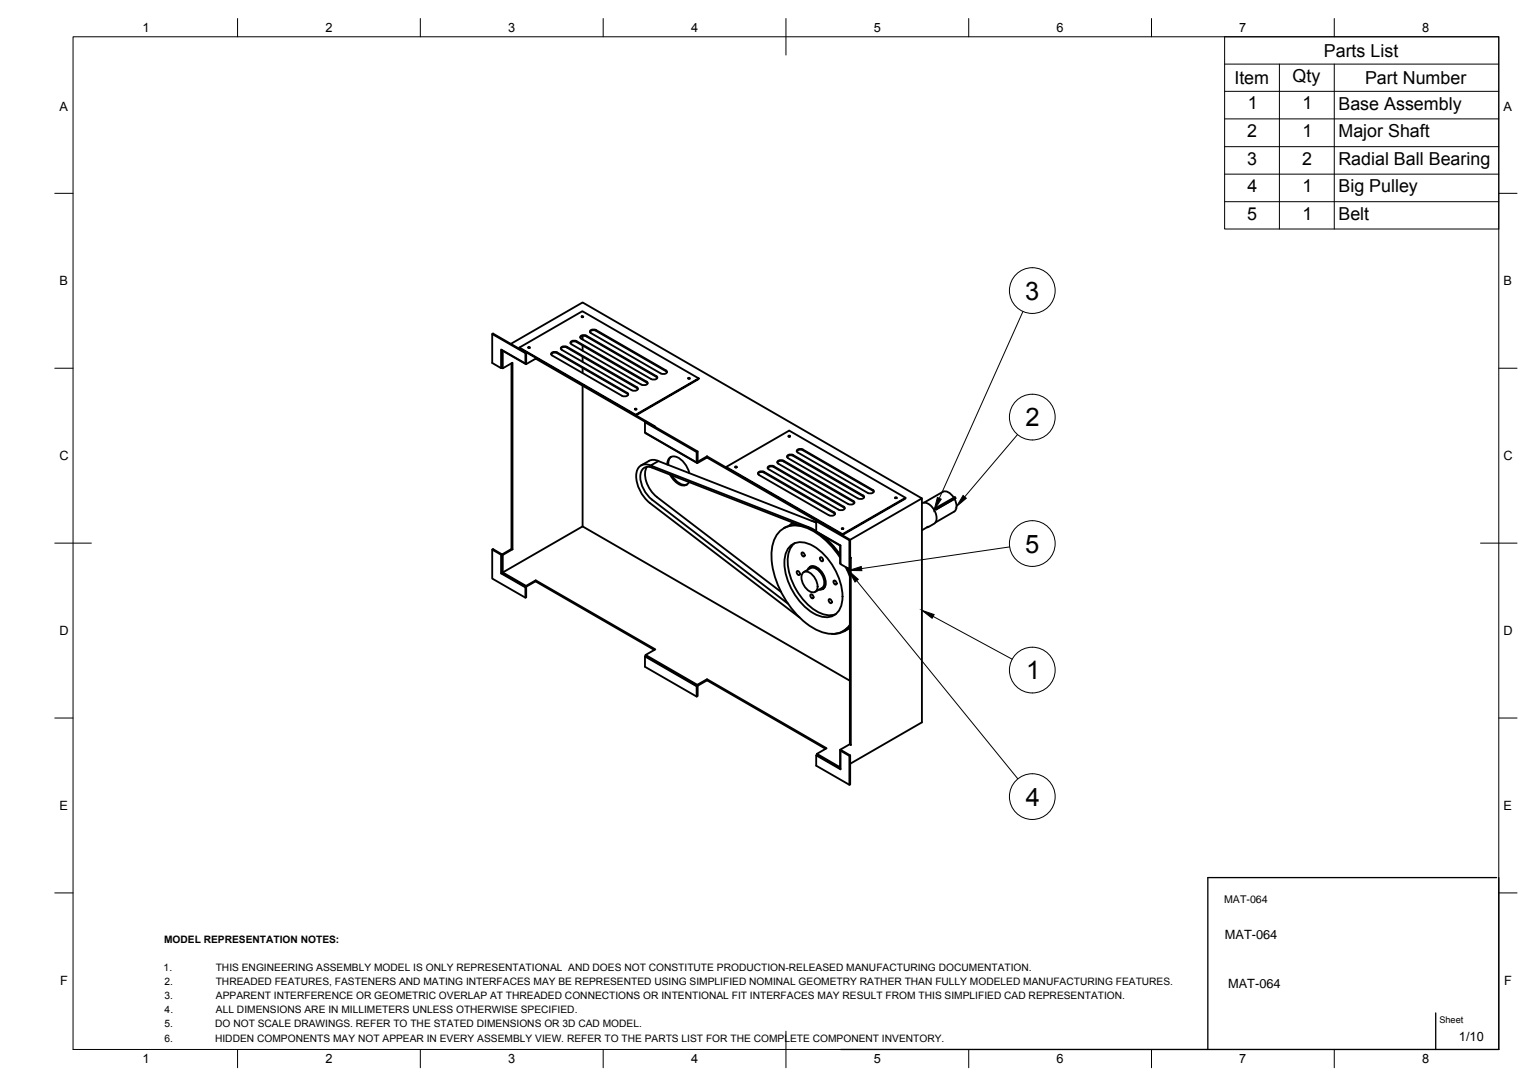
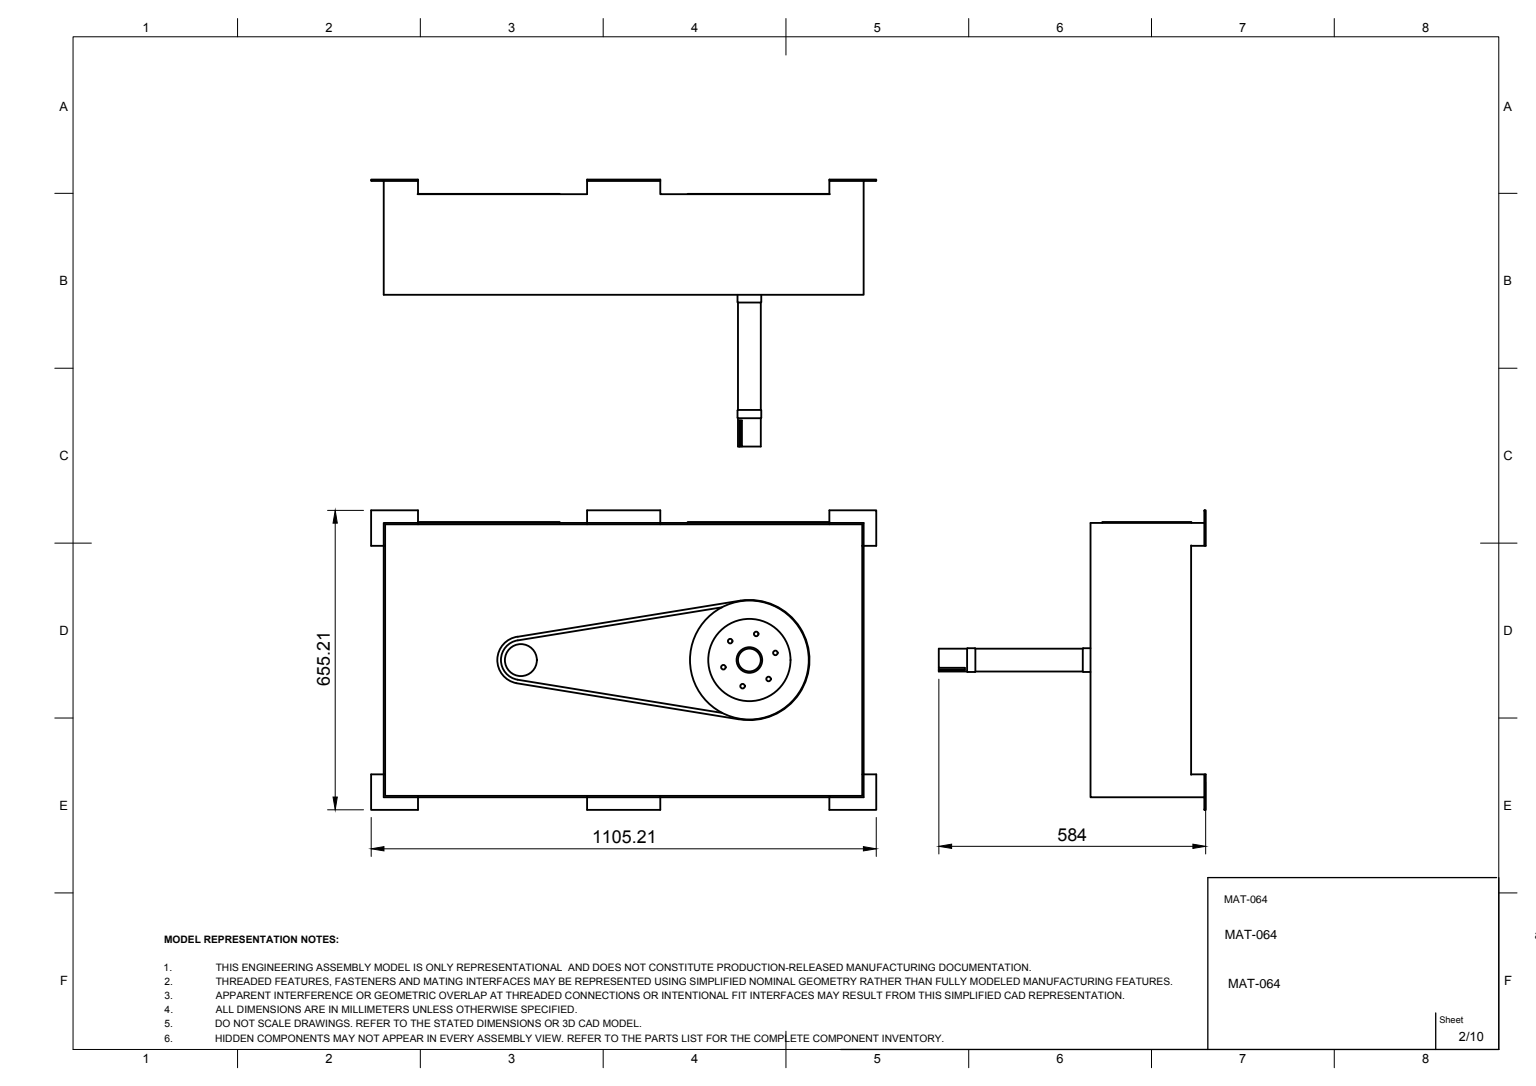
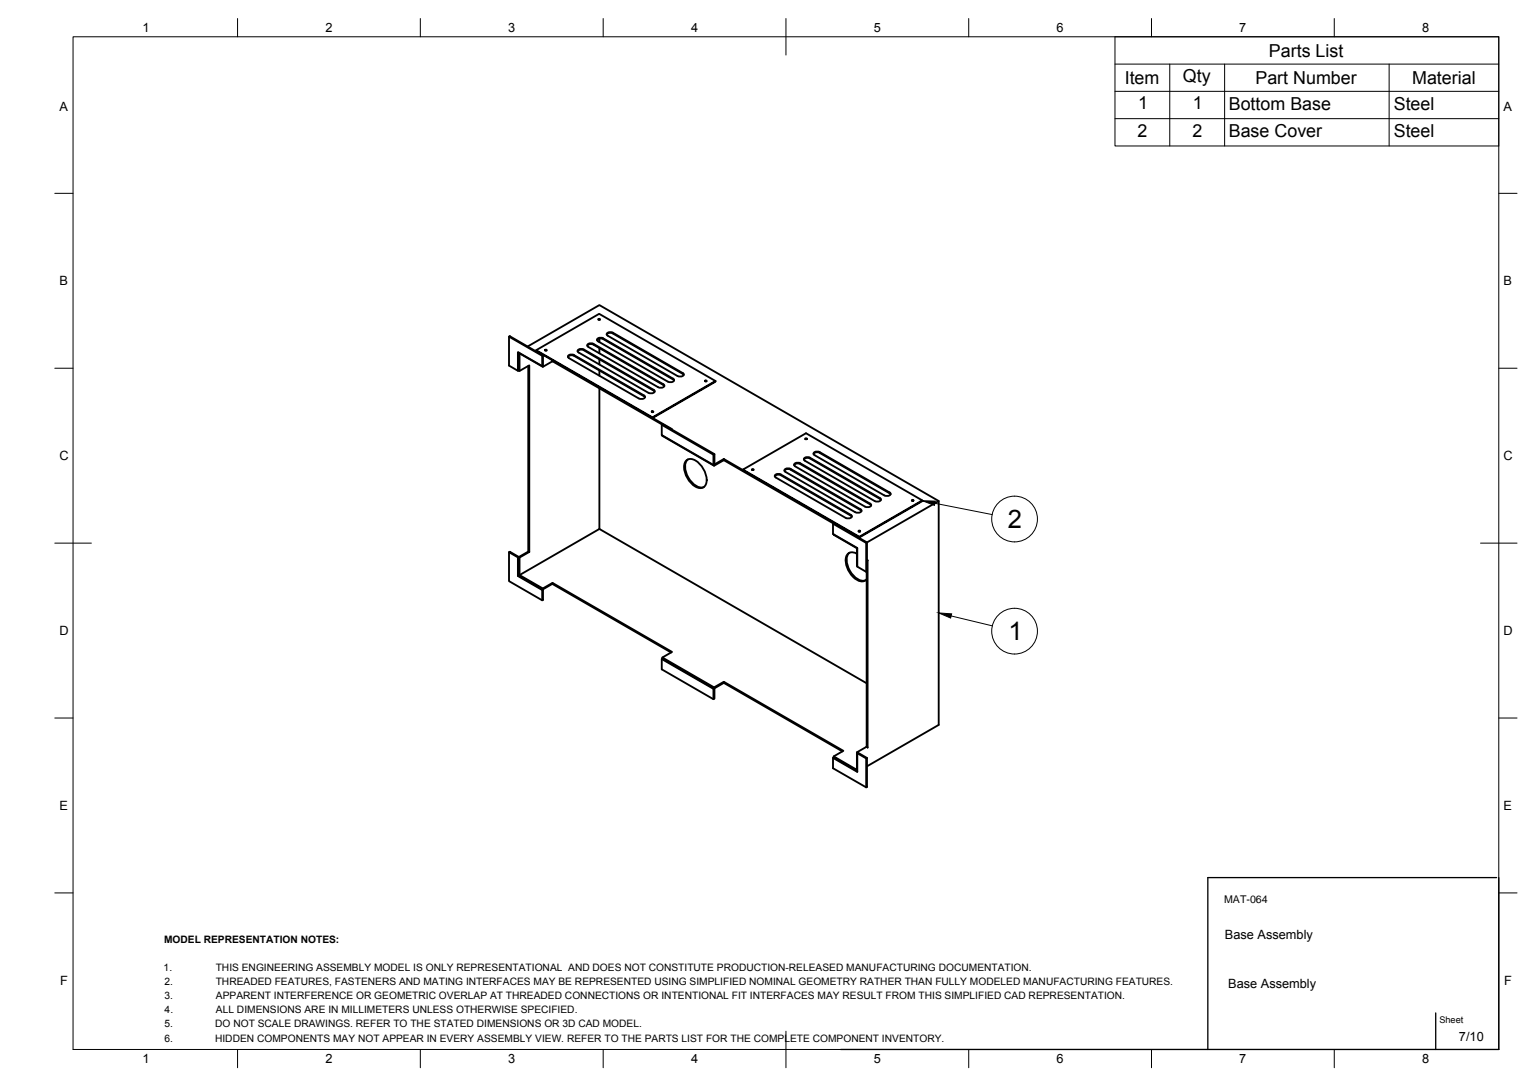
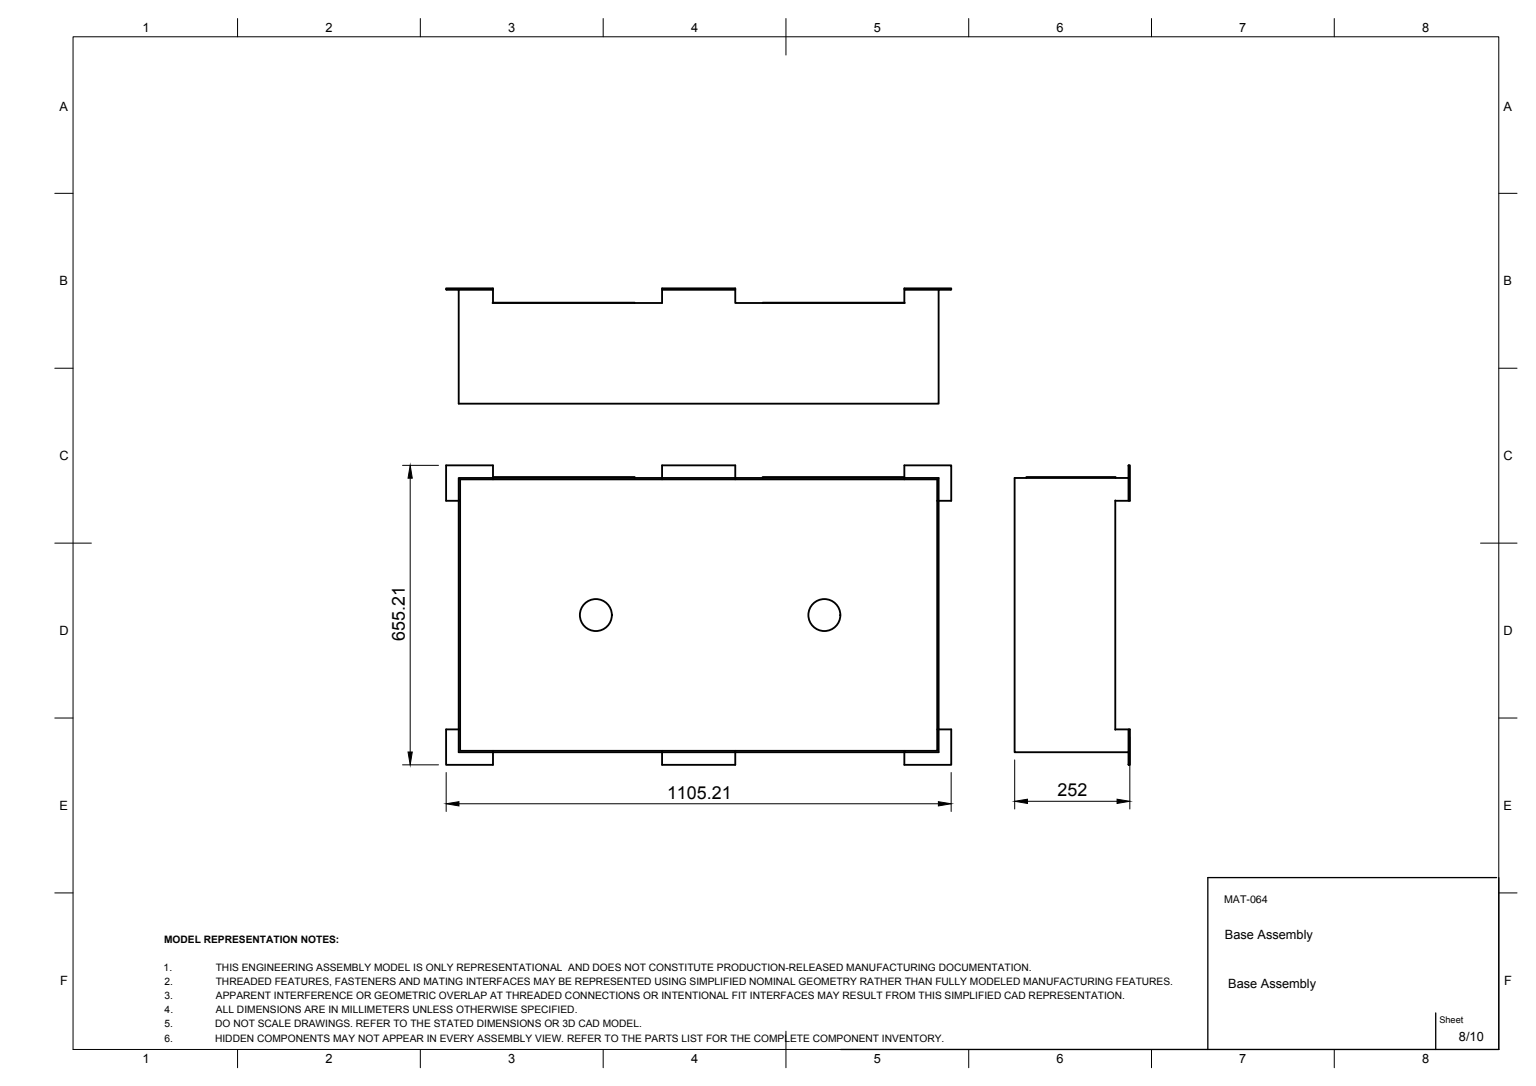
ISO-10303-21;
HEADER;
/* Generated by software containing ST-Developer
 * from STEP Tools, Inc. (www.steptools.com) 
 */

FILE_DESCRIPTION(
/* description */ (''),
/* implementation_level */ '2;1');

FILE_NAME(
/* name */ 
'MAT-064',
/* time_stamp */ '2026-10-24T12:42:14-07:00',
/* author */ (''),
/* organization */ (''),
/* preprocessor_version */ 'ST-DEVELOPER v20.2',
/* originating_system */ 'Autodesk Translation Framework v15.15.0.0',
/* authorisation */ '');

FILE_SCHEMA (('AUTOMOTIVE_DESIGN { 1 0 10303 214 3 1 1 }'));
ENDSEC;

DATA;
#10=MECHANICAL_DESIGN_GEOMETRIC_PRESENTATION_REPRESENTATION('',(#66,#67,
#68,#69,#70,#71),#6789);
#11=(
BOUNDED_SURFACE()
B_SPLINE_SURFACE(1,3,((#6689,#6690,#6691,#6692),(#6693,#6694,#6695,#6696)),
 .UNSPECIFIED.,.F.,.F.,.F.)
B_SPLINE_SURFACE_WITH_KNOTS((2,2),(4,4),(0.,1.),(0.,1.),.UNSPECIFIED.)
GEOMETRIC_REPRESENTATION_ITEM()
RATIONAL_B_SPLINE_SURFACE(((1.,0.44,0.44,1.),(1.,0.44,0.44,1.)))
REPRESENTATION_ITEM('')
SURFACE()
);
#12=(
BOUNDED_SURFACE()
B_SPLINE_SURFACE(1,3,((#6704,#6705,#6706,#6707),(#6708,#6709,#6710,#6711)),
 .UNSPECIFIED.,.F.,.F.,.F.)
B_SPLINE_SURFACE_WITH_KNOTS((2,2),(4,4),(0.,1.),(0.,1.),.UNSPECIFIED.)
GEOMETRIC_REPRESENTATION_ITEM()
RATIONAL_B_SPLINE_SURFACE(((1.,0.44,0.44,1.),(1.,0.44,0.44,1.)))
REPRESENTATION_ITEM('')
SURFACE()
);
#13=(
BOUNDED_SURFACE()
B_SPLINE_SURFACE(1,3,((#6733,#6734,#6735,#6736,#6737,#6738,#6739),(#6740,
#6741,#6742,#6743,#6744,#6745,#6746)),.UNSPECIFIED.,.F.,.F.,.F.)
B_SPLINE_SURFACE_WITH_KNOTS((2,2),(4,3,4),(0.,1.),(0.,0.5,1.),
 .UNSPECIFIED.)
GEOMETRIC_REPRESENTATION_ITEM()
RATIONAL_B_SPLINE_SURFACE(((1.,0.765382713227191,0.765382713227191,1.,0.765382713227191,
0.765382713227191,1.),(1.,0.765382713227191,0.765382713227191,1.,0.765382713227191,
0.765382713227191,1.)))
REPRESENTATION_ITEM('')
SURFACE()
);
#14=(
BOUNDED_SURFACE()
B_SPLINE_SURFACE(1,3,((#6750,#6751,#6752,#6753,#6754,#6755,#6756),(#6757,
#6758,#6759,#6760,#6761,#6762,#6763)),.UNSPECIFIED.,.F.,.F.,.F.)
B_SPLINE_SURFACE_WITH_KNOTS((2,2),(4,3,4),(0.,1.),(0.,0.5,1.),
 .UNSPECIFIED.)
GEOMETRIC_REPRESENTATION_ITEM()
RATIONAL_B_SPLINE_SURFACE(((1.,0.765382713227191,0.765382713227191,1.,0.765382713227191,
0.765382713227191,1.),(1.,0.765382713227191,0.765382713227191,1.,0.765382713227191,
0.765382713227191,1.)))
REPRESENTATION_ITEM('')
SURFACE()
);
#15=CONICAL_SURFACE('',#4306,7.5,0.0872664625997165);
#16=CONICAL_SURFACE('',#4399,122.,1.04719755119659);
#17=CONICAL_SURFACE('',#4402,130.,1.04719755119659);
#18=ITEM_DEFINED_TRANSFORMATION($,$,#4036,#4284);
#19=ITEM_DEFINED_TRANSFORMATION($,$,#4225,#4285);
#20=ITEM_DEFINED_TRANSFORMATION($,$,#4225,#4286);
#21=ITEM_DEFINED_TRANSFORMATION($,$,#4035,#4426);
#22=ITEM_DEFINED_TRANSFORMATION($,$,#4287,#4427);
#23=ITEM_DEFINED_TRANSFORMATION($,$,#4309,#4428);
#24=ITEM_DEFINED_TRANSFORMATION($,$,#4309,#4429);
#25=ITEM_DEFINED_TRANSFORMATION($,$,#4352,#4430);
#26=ITEM_DEFINED_TRANSFORMATION($,$,#4405,#4431);
#27=(
REPRESENTATION_RELATIONSHIP($,$,#6821,#6820)
REPRESENTATION_RELATIONSHIP_WITH_TRANSFORMATION(#18)
SHAPE_REPRESENTATION_RELATIONSHIP()
);
#28=(
REPRESENTATION_RELATIONSHIP($,$,#6822,#6820)
REPRESENTATION_RELATIONSHIP_WITH_TRANSFORMATION(#19)
SHAPE_REPRESENTATION_RELATIONSHIP()
);
#29=(
REPRESENTATION_RELATIONSHIP($,$,#6822,#6820)
REPRESENTATION_RELATIONSHIP_WITH_TRANSFORMATION(#20)
SHAPE_REPRESENTATION_RELATIONSHIP()
);
#30=(
REPRESENTATION_RELATIONSHIP($,$,#6820,#6819)
REPRESENTATION_RELATIONSHIP_WITH_TRANSFORMATION(#21)
SHAPE_REPRESENTATION_RELATIONSHIP()
);
#31=(
REPRESENTATION_RELATIONSHIP($,$,#6823,#6819)
REPRESENTATION_RELATIONSHIP_WITH_TRANSFORMATION(#22)
SHAPE_REPRESENTATION_RELATIONSHIP()
);
#32=(
REPRESENTATION_RELATIONSHIP($,$,#6824,#6819)
REPRESENTATION_RELATIONSHIP_WITH_TRANSFORMATION(#23)
SHAPE_REPRESENTATION_RELATIONSHIP()
);
#33=(
REPRESENTATION_RELATIONSHIP($,$,#6824,#6819)
REPRESENTATION_RELATIONSHIP_WITH_TRANSFORMATION(#24)
SHAPE_REPRESENTATION_RELATIONSHIP()
);
#34=(
REPRESENTATION_RELATIONSHIP($,$,#6825,#6819)
REPRESENTATION_RELATIONSHIP_WITH_TRANSFORMATION(#25)
SHAPE_REPRESENTATION_RELATIONSHIP()
);
#35=(
REPRESENTATION_RELATIONSHIP($,$,#6826,#6819)
REPRESENTATION_RELATIONSHIP_WITH_TRANSFORMATION(#26)
SHAPE_REPRESENTATION_RELATIONSHIP()
);
#36=CONTEXT_DEPENDENT_SHAPE_REPRESENTATION(#27,#6806);
#37=CONTEXT_DEPENDENT_SHAPE_REPRESENTATION(#28,#6807);
#38=CONTEXT_DEPENDENT_SHAPE_REPRESENTATION(#29,#6808);
#39=CONTEXT_DEPENDENT_SHAPE_REPRESENTATION(#30,#6813);
#40=CONTEXT_DEPENDENT_SHAPE_REPRESENTATION(#31,#6814);
#41=CONTEXT_DEPENDENT_SHAPE_REPRESENTATION(#32,#6815);
#42=CONTEXT_DEPENDENT_SHAPE_REPRESENTATION(#33,#6816);
#43=CONTEXT_DEPENDENT_SHAPE_REPRESENTATION(#34,#6817);
#44=CONTEXT_DEPENDENT_SHAPE_REPRESENTATION(#35,#6818);
#45=NEXT_ASSEMBLY_USAGE_OCCURRENCE('Bottom Base:1','Bottom Base:1',
'Bottom Base:1',#6829,#6830,'Bottom Base:1');
#46=NEXT_ASSEMBLY_USAGE_OCCURRENCE('Base Cover:1','Base Cover:1',
'Base Cover:1',#6829,#6831,'Base Cover:1');
#47=NEXT_ASSEMBLY_USAGE_OCCURRENCE('Base Cover:2','Base Cover:2',
'Base Cover:2',#6829,#6831,'Base Cover:2');
#48=NEXT_ASSEMBLY_USAGE_OCCURRENCE('Base Assembly:1','Base Assembly:1',
'Base Assembly:1',#6828,#6829,'Base Assembly:1');
#49=NEXT_ASSEMBLY_USAGE_OCCURRENCE('Major Shaft:1','Major Shaft:1',
'Major Shaft:1',#6828,#6832,'Major Shaft:1');
#50=NEXT_ASSEMBLY_USAGE_OCCURRENCE('Radial Ball Bearing:1',
'Radial Ball Bearing:1','Radial Ball Bearing:1',#6828,#6833,
'Radial Ball Bearing:1');
#51=NEXT_ASSEMBLY_USAGE_OCCURRENCE('Radial Ball Bearing:2',
'Radial Ball Bearing:2','Radial Ball Bearing:2',#6828,#6833,
'Radial Ball Bearing:2');
#52=NEXT_ASSEMBLY_USAGE_OCCURRENCE('Big Pulley:1','Big Pulley:1',
'Big Pulley:1',#6828,#6834,'Big Pulley:1');
#53=NEXT_ASSEMBLY_USAGE_OCCURRENCE('Belt:1','Belt:1','Belt:1',#6828,#6835,
'Belt:1');
#54=SHAPE_REPRESENTATION_RELATIONSHIP('SRR','None',#6821,#60);
#55=SHAPE_REPRESENTATION_RELATIONSHIP('SRR','None',#6822,#61);
#56=SHAPE_REPRESENTATION_RELATIONSHIP('SRR','None',#6823,#62);
#57=SHAPE_REPRESENTATION_RELATIONSHIP('SRR','None',#6824,#63);
#58=SHAPE_REPRESENTATION_RELATIONSHIP('SRR','None',#6825,#64);
#59=SHAPE_REPRESENTATION_RELATIONSHIP('SRR','None',#6826,#65);
#60=ADVANCED_BREP_SHAPE_REPRESENTATION('',(#72),#6783);
#61=ADVANCED_BREP_SHAPE_REPRESENTATION('',(#73),#6784);
#62=ADVANCED_BREP_SHAPE_REPRESENTATION('',(#74),#6785);
#63=ADVANCED_BREP_SHAPE_REPRESENTATION('',(#75),#6786);
#64=ADVANCED_BREP_SHAPE_REPRESENTATION('',(#76),#6787);
#65=ADVANCED_BREP_SHAPE_REPRESENTATION('',(#77),#6788);
#66=STYLED_ITEM('',(#6863),#72);
#67=STYLED_ITEM('',(#6863),#73);
#68=STYLED_ITEM('',(#6863),#74);
#69=STYLED_ITEM('',(#6863),#75);
#70=STYLED_ITEM('',(#6864),#76);
#71=STYLED_ITEM('',(#6863),#77);
#72=MANIFOLD_SOLID_BREP('Bottom Base',#3961);
#73=MANIFOLD_SOLID_BREP('Base Cover',#3962);
#74=MANIFOLD_SOLID_BREP('Major Shaft',#3963);
#75=MANIFOLD_SOLID_BREP('Radial Ball Bearing',#3964);
#76=MANIFOLD_SOLID_BREP('Big Pulley',#3965);
#77=MANIFOLD_SOLID_BREP('Belt',#3966);
#78=TOROIDAL_SURFACE('',#4150,2.,1.);
#79=TOROIDAL_SURFACE('',#4160,2.,1.);
#80=TOROIDAL_SURFACE('',#4170,2.,1.);
#81=TOROIDAL_SURFACE('',#4180,2.,1.);
#82=TOROIDAL_SURFACE('',#4190,2.,1.);
#83=TOROIDAL_SURFACE('',#4200,2.,1.);
#84=TOROIDAL_SURFACE('',#4208,2.,1.);
#85=TOROIDAL_SURFACE('',#4220,2.,1.);
#86=TOROIDAL_SURFACE('',#4310,19.25,4.05);
#87=TOROIDAL_SURFACE('',#4324,13.5,1.);
#88=TOROIDAL_SURFACE('',#4329,13.5,1.);
#89=TOROIDAL_SURFACE('',#4333,19.25,4.05);
#90=TOROIDAL_SURFACE('',#4343,25.,0.999999999999999);
#91=TOROIDAL_SURFACE('',#4348,25.,0.999999999999999);
#92=ELLIPSE('',#4145,1.41421356237309,1.);
#93=ELLIPSE('',#4149,1.41421356237309,1.);
#94=ELLIPSE('',#4153,1.41421356237309,1.);
#95=ELLIPSE('',#4155,1.41421356237309,1.);
#96=ELLIPSE('',#4165,1.4142135623731,1.);
#97=ELLIPSE('',#4169,1.41421356237309,1.);
#98=ELLIPSE('',#4173,1.41421356237309,1.);
#99=ELLIPSE('',#4175,1.41421356237309,1.);
#100=ELLIPSE('',#4185,1.41421356237309,1.);
#101=ELLIPSE('',#4189,1.41421356237309,1.);
#102=ELLIPSE('',#4193,1.41421356237309,1.);
#103=ELLIPSE('',#4195,1.41421356237309,1.);
#104=ELLIPSE('',#4206,1.41421356237309,1.);
#105=ELLIPSE('',#4211,1.41421356237309,1.);
#106=ELLIPSE('',#4213,1.4142135623731,1.);
#107=ELLIPSE('',#4215,1.4142135623731,1.);
#108=CYLINDRICAL_SURFACE('',#4093,2.);
#109=CYLINDRICAL_SURFACE('',#4094,2.);
#110=CYLINDRICAL_SURFACE('',#4095,2.);
#111=CYLINDRICAL_SURFACE('',#4096,2.);
#112=CYLINDRICAL_SURFACE('',#4143,1.);
#113=CYLINDRICAL_SURFACE('',#4146,1.);
#114=CYLINDRICAL_SURFACE('',#4148,1.);
#115=CYLINDRICAL_SURFACE('',#4152,1.);
#116=CYLINDRICAL_SURFACE('',#4154,1.);
#117=CYLINDRICAL_SURFACE('',#4156,1.);
#118=CYLINDRICAL_SURFACE('',#4158,1.);
#119=CYLINDRICAL_SURFACE('',#4162,1.);
#120=CYLINDRICAL_SURFACE('',#4163,1.);
#121=CYLINDRICAL_SURFACE('',#4166,1.);
#122=CYLINDRICAL_SURFACE('',#4168,1.);
#123=CYLINDRICAL_SURFACE('',#4172,1.);
#124=CYLINDRICAL_SURFACE('',#4174,1.);
#125=CYLINDRICAL_SURFACE('',#4176,1.);
#126=CYLINDRICAL_SURFACE('',#4178,1.);
#127=CYLINDRICAL_SURFACE('',#4182,1.);
#128=CYLINDRICAL_SURFACE('',#4183,1.);
#129=CYLINDRICAL_SURFACE('',#4186,1.);
#130=CYLINDRICAL_SURFACE('',#4188,1.);
#131=CYLINDRICAL_SURFACE('',#4192,1.);
#132=CYLINDRICAL_SURFACE('',#4194,1.);
#133=CYLINDRICAL_SURFACE('',#4196,1.);
#134=CYLINDRICAL_SURFACE('',#4198,1.);
#135=CYLINDRICAL_SURFACE('',#4202,1.);
#136=CYLINDRICAL_SURFACE('',#4203,1.);
#137=CYLINDRICAL_SURFACE('',#4205,1.);
#138=CYLINDRICAL_SURFACE('',#4210,1.);
#139=CYLINDRICAL_SURFACE('',#4212,1.);
#140=CYLINDRICAL_SURFACE('',#4214,1.);
#141=CYLINDRICAL_SURFACE('',#4216,1.);
#142=CYLINDRICAL_SURFACE('',#4218,1.);
#143=CYLINDRICAL_SURFACE('',#4222,1.);
#144=CYLINDRICAL_SURFACE('',#4223,35.);
#145=CYLINDRICAL_SURFACE('',#4224,35.);
#146=CYLINDRICAL_SURFACE('',#4260,2.);
#147=CYLINDRICAL_SURFACE('',#4261,2.);
#148=CYLINDRICAL_SURFACE('',#4262,2.);
#149=CYLINDRICAL_SURFACE('',#4263,2.);
#150=CYLINDRICAL_SURFACE('',#4264,7.99999999999998);
#151=CYLINDRICAL_SURFACE('',#4266,8.00000000000009);
#152=CYLINDRICAL_SURFACE('',#4268,8.00000000000009);
#153=CYLINDRICAL_SURFACE('',#4270,8.00000000000004);
#154=CYLINDRICAL_SURFACE('',#4272,7.99999999999998);
#155=CYLINDRICAL_SURFACE('',#4274,8.00000000000009);
#156=CYLINDRICAL_SURFACE('',#4276,8.00000000000009);
#157=CYLINDRICAL_SURFACE('',#4278,8.00000000000004);
#158=CYLINDRICAL_SURFACE('',#4280,8.00000000000004);
#159=CYLINDRICAL_SURFACE('',#4282,8.00000000000004);
#160=CYLINDRICAL_SURFACE('',#4288,25.);
#161=CYLINDRICAL_SURFACE('',#4316,16.55);
#162=CYLINDRICAL_SURFACE('',#4318,16.55);
#163=CYLINDRICAL_SURFACE('',#4327,12.5);
#164=CYLINDRICAL_SURFACE('',#4337,21.95);
#165=CYLINDRICAL_SURFACE('',#4339,21.95);
#166=CYLINDRICAL_SURFACE('',#4346,26.);
#167=CYLINDRICAL_SURFACE('',#4353,130.);
#168=CYLINDRICAL_SURFACE('',#4356,130.);
#169=CYLINDRICAL_SURFACE('',#4360,5.);
#170=CYLINDRICAL_SURFACE('',#4363,5.);
#171=CYLINDRICAL_SURFACE('',#4366,5.);
#172=CYLINDRICAL_SURFACE('',#4369,5.);
#173=CYLINDRICAL_SURFACE('',#4372,5.);
#174=CYLINDRICAL_SURFACE('',#4375,90.);
#175=CYLINDRICAL_SURFACE('',#4378,90.);
#176=CYLINDRICAL_SURFACE('',#4389,28.);
#177=CYLINDRICAL_SURFACE('',#4391,25.);
#178=CYLINDRICAL_SURFACE('',#4394,28.);
#179=CYLINDRICAL_SURFACE('',#4398,5.);
#180=CYLINDRICAL_SURFACE('',#4404,122.);
#181=CYLINDRICAL_SURFACE('',#4409,51.471200702168);
#182=CYLINDRICAL_SURFACE('',#4413,43.5522017822105);
#183=CYLINDRICAL_SURFACE('',#4419,131.457333002004);
#184=CYLINDRICAL_SURFACE('',#4423,123.55173167544);
#185=FACE_BOUND('',#612,.T.);
#186=FACE_BOUND('',#613,.T.);
#187=FACE_BOUND('',#614,.T.);
#188=FACE_BOUND('',#615,.T.);
#189=FACE_BOUND('',#616,.T.);
#190=FACE_BOUND('',#617,.T.);
#191=FACE_BOUND('',#624,.T.);
#192=FACE_BOUND('',#625,.T.);
#193=FACE_BOUND('',#626,.T.);
#194=FACE_BOUND('',#627,.T.);
#195=FACE_BOUND('',#628,.T.);
#196=FACE_BOUND('',#629,.T.);
#197=FACE_BOUND('',#635,.T.);
#198=FACE_BOUND('',#636,.T.);
#199=FACE_BOUND('',#641,.T.);
#200=FACE_BOUND('',#642,.T.);
#201=FACE_BOUND('',#752,.T.);
#202=FACE_BOUND('',#753,.T.);
#203=FACE_BOUND('',#754,.T.);
#204=FACE_BOUND('',#755,.T.);
#205=FACE_BOUND('',#756,.T.);
#206=FACE_BOUND('',#757,.T.);
#207=FACE_BOUND('',#758,.T.);
#208=FACE_BOUND('',#759,.T.);
#209=FACE_BOUND('',#760,.T.);
#210=FACE_BOUND('',#762,.T.);
#211=FACE_BOUND('',#763,.T.);
#212=FACE_BOUND('',#764,.T.);
#213=FACE_BOUND('',#765,.T.);
#214=FACE_BOUND('',#766,.T.);
#215=FACE_BOUND('',#767,.T.);
#216=FACE_BOUND('',#768,.T.);
#217=FACE_BOUND('',#769,.T.);
#218=FACE_BOUND('',#770,.T.);
#219=FACE_BOUND('',#797,.T.);
#220=FACE_BOUND('',#813,.T.);
#221=FACE_BOUND('',#818,.T.);
#222=FACE_BOUND('',#823,.T.);
#223=FACE_BOUND('',#828,.T.);
#224=FACE_BOUND('',#839,.T.);
#225=FACE_BOUND('',#841,.T.);
#226=FACE_BOUND('',#843,.T.);
#227=FACE_BOUND('',#844,.T.);
#228=FACE_BOUND('',#845,.T.);
#229=FACE_BOUND('',#846,.T.);
#230=FACE_BOUND('',#847,.T.);
#231=FACE_BOUND('',#848,.T.);
#232=FACE_BOUND('',#849,.T.);
#233=FACE_BOUND('',#851,.T.);
#234=FACE_BOUND('',#852,.T.);
#235=FACE_BOUND('',#853,.T.);
#236=FACE_BOUND('',#854,.T.);
#237=FACE_BOUND('',#855,.T.);
#238=FACE_BOUND('',#856,.T.);
#239=FACE_BOUND('',#857,.T.);
#240=FACE_BOUND('',#862,.T.);
#241=FACE_BOUND('',#864,.T.);
#242=CIRCLE('',#4038,2.);
#243=CIRCLE('',#4039,2.);
#244=CIRCLE('',#4040,2.);
#245=CIRCLE('',#4041,2.);
#246=CIRCLE('',#4048,2.);
#247=CIRCLE('',#4049,2.);
#248=CIRCLE('',#4050,2.);
#249=CIRCLE('',#4051,2.);
#250=CIRCLE('',#4057,35.);
#251=CIRCLE('',#4058,35.);
#252=CIRCLE('',#4063,35.);
#253=CIRCLE('',#4064,35.);
#254=CIRCLE('',#4067,1.);
#255=CIRCLE('',#4069,2.);
#256=CIRCLE('',#4071,2.);
#257=CIRCLE('',#4073,1.);
#258=CIRCLE('',#4077,1.);
#259=CIRCLE('',#4079,2.);
#260=CIRCLE('',#4082,2.);
#261=CIRCLE('',#4084,1.);
#262=CIRCLE('',#4098,2.);
#263=CIRCLE('',#4100,1.);
#264=CIRCLE('',#4101,1.);
#265=CIRCLE('',#4103,2.);
#266=CIRCLE('',#4105,2.);
#267=CIRCLE('',#4107,1.);
#268=CIRCLE('',#4108,1.);
#269=CIRCLE('',#4110,2.);
#270=CIRCLE('',#4144,1.);
#271=CIRCLE('',#4147,1.);
#272=CIRCLE('',#4151,1.);
#273=CIRCLE('',#4157,1.);
#274=CIRCLE('',#4159,1.);
#275=CIRCLE('',#4161,1.);
#276=CIRCLE('',#4164,1.);
#277=CIRCLE('',#4167,1.);
#278=CIRCLE('',#4171,1.);
#279=CIRCLE('',#4177,1.);
#280=CIRCLE('',#4179,1.);
#281=CIRCLE('',#4181,1.);
#282=CIRCLE('',#4184,1.);
#283=CIRCLE('',#4187,1.);
#284=CIRCLE('',#4191,1.);
#285=CIRCLE('',#4197,1.);
#286=CIRCLE('',#4199,1.);
#287=CIRCLE('',#4201,1.);
#288=CIRCLE('',#4204,1.);
#289=CIRCLE('',#4207,1.);
#290=CIRCLE('',#4209,1.);
#291=CIRCLE('',#4217,1.);
#292=CIRCLE('',#4219,1.);
#293=CIRCLE('',#4221,1.);
#294=CIRCLE('',#4231,8.00000000000004);
#295=CIRCLE('',#4232,8.00000000000004);
#296=CIRCLE('',#4233,8.00000000000009);
#297=CIRCLE('',#4234,8.00000000000004);
#298=CIRCLE('',#4235,7.99999999999998);
#299=CIRCLE('',#4236,8.00000000000009);
#300=CIRCLE('',#4237,8.00000000000009);
#301=CIRCLE('',#4238,8.00000000000004);
#302=CIRCLE('',#4239,7.99999999999998);
#303=CIRCLE('',#4240,8.00000000000009);
#304=CIRCLE('',#4241,2.);
#305=CIRCLE('',#4242,2.);
#306=CIRCLE('',#4243,2.);
#307=CIRCLE('',#4244,2.);
#308=CIRCLE('',#4246,8.00000000000004);
#309=CIRCLE('',#4247,8.00000000000004);
#310=CIRCLE('',#4248,8.00000000000009);
#311=CIRCLE('',#4249,8.00000000000004);
#312=CIRCLE('',#4250,7.99999999999998);
#313=CIRCLE('',#4251,8.00000000000009);
#314=CIRCLE('',#4252,8.00000000000009);
#315=CIRCLE('',#4253,8.00000000000004);
#316=CIRCLE('',#4254,7.99999999999998);
#317=CIRCLE('',#4255,8.00000000000009);
#318=CIRCLE('',#4256,2.);
#319=CIRCLE('',#4257,2.);
#320=CIRCLE('',#4258,2.);
#321=CIRCLE('',#4259,2.);
#322=CIRCLE('',#4289,25.);
#323=CIRCLE('',#4290,25.);
#324=CIRCLE('',#4291,25.);
#325=CIRCLE('',#4292,25.);
#326=CIRCLE('',#4293,25.);
#327=CIRCLE('',#4294,25.);
#328=CIRCLE('',#4296,7.5);
#329=CIRCLE('',#4307,4.87534009422228);
#330=CIRCLE('',#4311,21.95);
#331=CIRCLE('',#4312,4.05);
#332=CIRCLE('',#4313,16.55);
#333=CIRCLE('',#4314,16.55);
#334=CIRCLE('',#4315,21.95);
#335=CIRCLE('',#4317,16.55);
#336=CIRCLE('',#4319,16.55);
#337=CIRCLE('',#4320,16.55);
#338=CIRCLE('',#4321,16.55);
#339=CIRCLE('',#4323,13.5);
#340=CIRCLE('',#4325,12.5);
#341=CIRCLE('',#4326,1.);
#342=CIRCLE('',#4328,12.5);
#343=CIRCLE('',#4330,13.5);
#344=CIRCLE('',#4331,1.);
#345=CIRCLE('',#4334,4.05);
#346=CIRCLE('',#4335,21.95);
#347=CIRCLE('',#4336,21.95);
#348=CIRCLE('',#4338,21.95);
#349=CIRCLE('',#4340,21.95);
#350=CIRCLE('',#4342,25.);
#351=CIRCLE('',#4344,0.999999999999999);
#352=CIRCLE('',#4345,26.);
#353=CIRCLE('',#4347,26.);
#354=CIRCLE('',#4349,0.999999999999999);
#355=CIRCLE('',#4350,25.);
#356=CIRCLE('',#4354,130.);
#357=CIRCLE('',#4355,130.);
#358=CIRCLE('',#4357,130.);
#359=CIRCLE('',#4358,130.);
#360=CIRCLE('',#4359,130.);
#361=CIRCLE('',#4361,5.);
#362=CIRCLE('',#4362,5.);
#363=CIRCLE('',#4364,5.);
#364=CIRCLE('',#4365,5.);
#365=CIRCLE('',#4367,5.);
#366=CIRCLE('',#4368,5.);
#367=CIRCLE('',#4370,5.);
#368=CIRCLE('',#4371,5.);
#369=CIRCLE('',#4373,5.);
#370=CIRCLE('',#4374,5.);
#371=CIRCLE('',#4376,90.);
#372=CIRCLE('',#4377,90.);
#373=CIRCLE('',#4379,90.);
#374=CIRCLE('',#4380,90.);
#375=CIRCLE('',#4384,5.);
#376=CIRCLE('',#4385,28.);
#377=CIRCLE('',#4387,5.);
#378=CIRCLE('',#4388,28.);
#379=CIRCLE('',#4390,28.);
#380=CIRCLE('',#4392,25.);
#381=CIRCLE('',#4393,25.);
#382=CIRCLE('',#4395,28.);
#383=CIRCLE('',#4400,122.);
#384=CIRCLE('',#4401,122.);
#385=CIRCLE('',#4403,122.);
#386=CIRCLE('',#4410,51.471200702168);
#387=CIRCLE('',#4411,51.471200702168);
#388=CIRCLE('',#4412,43.5522017822105);
#389=CIRCLE('',#4414,43.5522017822105);
#390=CIRCLE('',#4420,131.457333002004);
#391=CIRCLE('',#4421,131.457333002004);
#392=CIRCLE('',#4422,123.55173167544);
#393=CIRCLE('',#4424,123.55173167544);
#394=FACE_OUTER_BOUND('',#611,.T.);
#395=FACE_OUTER_BOUND('',#618,.T.);
#396=FACE_OUTER_BOUND('',#619,.T.);
#397=FACE_OUTER_BOUND('',#620,.T.);
#398=FACE_OUTER_BOUND('',#621,.T.);
#399=FACE_OUTER_BOUND('',#622,.T.);
#400=FACE_OUTER_BOUND('',#623,.T.);
#401=FACE_OUTER_BOUND('',#630,.T.);
#402=FACE_OUTER_BOUND('',#631,.T.);
#403=FACE_OUTER_BOUND('',#632,.T.);
#404=FACE_OUTER_BOUND('',#633,.T.);
#405=FACE_OUTER_BOUND('',#634,.T.);
#406=FACE_OUTER_BOUND('',#637,.T.);
#407=FACE_OUTER_BOUND('',#638,.T.);
#408=FACE_OUTER_BOUND('',#639,.T.);
#409=FACE_OUTER_BOUND('',#640,.T.);
#410=FACE_OUTER_BOUND('',#643,.T.);
#411=FACE_OUTER_BOUND('',#644,.T.);
#412=FACE_OUTER_BOUND('',#645,.T.);
#413=FACE_OUTER_BOUND('',#646,.T.);
#414=FACE_OUTER_BOUND('',#647,.T.);
#415=FACE_OUTER_BOUND('',#648,.T.);
#416=FACE_OUTER_BOUND('',#649,.T.);
#417=FACE_OUTER_BOUND('',#650,.T.);
#418=FACE_OUTER_BOUND('',#651,.T.);
#419=FACE_OUTER_BOUND('',#652,.T.);
#420=FACE_OUTER_BOUND('',#653,.T.);
#421=FACE_OUTER_BOUND('',#654,.T.);
#422=FACE_OUTER_BOUND('',#655,.T.);
#423=FACE_OUTER_BOUND('',#656,.T.);
#424=FACE_OUTER_BOUND('',#657,.T.);
#425=FACE_OUTER_BOUND('',#658,.T.);
#426=FACE_OUTER_BOUND('',#659,.T.);
#427=FACE_OUTER_BOUND('',#660,.T.);
#428=FACE_OUTER_BOUND('',#661,.T.);
#429=FACE_OUTER_BOUND('',#662,.T.);
#430=FACE_OUTER_BOUND('',#663,.T.);
#431=FACE_OUTER_BOUND('',#664,.T.);
#432=FACE_OUTER_BOUND('',#665,.T.);
#433=FACE_OUTER_BOUND('',#666,.T.);
#434=FACE_OUTER_BOUND('',#667,.T.);
#435=FACE_OUTER_BOUND('',#668,.T.);
#436=FACE_OUTER_BOUND('',#669,.T.);
#437=FACE_OUTER_BOUND('',#670,.T.);
#438=FACE_OUTER_BOUND('',#671,.T.);
#439=FACE_OUTER_BOUND('',#672,.T.);
#440=FACE_OUTER_BOUND('',#673,.T.);
#441=FACE_OUTER_BOUND('',#674,.T.);
#442=FACE_OUTER_BOUND('',#675,.T.);
#443=FACE_OUTER_BOUND('',#676,.T.);
#444=FACE_OUTER_BOUND('',#677,.T.);
#445=FACE_OUTER_BOUND('',#678,.T.);
#446=FACE_OUTER_BOUND('',#679,.T.);
#447=FACE_OUTER_BOUND('',#680,.T.);
#448=FACE_OUTER_BOUND('',#681,.T.);
#449=FACE_OUTER_BOUND('',#682,.T.);
#450=FACE_OUTER_BOUND('',#683,.T.);
#451=FACE_OUTER_BOUND('',#684,.T.);
#452=FACE_OUTER_BOUND('',#685,.T.);
#453=FACE_OUTER_BOUND('',#686,.T.);
#454=FACE_OUTER_BOUND('',#687,.T.);
#455=FACE_OUTER_BOUND('',#688,.T.);
#456=FACE_OUTER_BOUND('',#689,.T.);
#457=FACE_OUTER_BOUND('',#690,.T.);
#458=FACE_OUTER_BOUND('',#691,.T.);
#459=FACE_OUTER_BOUND('',#692,.T.);
#460=FACE_OUTER_BOUND('',#693,.T.);
#461=FACE_OUTER_BOUND('',#694,.T.);
#462=FACE_OUTER_BOUND('',#695,.T.);
#463=FACE_OUTER_BOUND('',#696,.T.);
#464=FACE_OUTER_BOUND('',#697,.T.);
#465=FACE_OUTER_BOUND('',#698,.T.);
#466=FACE_OUTER_BOUND('',#699,.T.);
#467=FACE_OUTER_BOUND('',#700,.T.);
#468=FACE_OUTER_BOUND('',#701,.T.);
#469=FACE_OUTER_BOUND('',#702,.T.);
#470=FACE_OUTER_BOUND('',#703,.T.);
#471=FACE_OUTER_BOUND('',#704,.T.);
#472=FACE_OUTER_BOUND('',#705,.T.);
#473=FACE_OUTER_BOUND('',#706,.T.);
#474=FACE_OUTER_BOUND('',#707,.T.);
#475=FACE_OUTER_BOUND('',#708,.T.);
#476=FACE_OUTER_BOUND('',#709,.T.);
#477=FACE_OUTER_BOUND('',#710,.T.);
#478=FACE_OUTER_BOUND('',#711,.T.);
#479=FACE_OUTER_BOUND('',#712,.T.);
#480=FACE_OUTER_BOUND('',#713,.T.);
#481=FACE_OUTER_BOUND('',#714,.T.);
#482=FACE_OUTER_BOUND('',#715,.T.);
#483=FACE_OUTER_BOUND('',#716,.T.);
#484=FACE_OUTER_BOUND('',#717,.T.);
#485=FACE_OUTER_BOUND('',#718,.T.);
#486=FACE_OUTER_BOUND('',#719,.T.);
#487=FACE_OUTER_BOUND('',#720,.T.);
#488=FACE_OUTER_BOUND('',#721,.T.);
#489=FACE_OUTER_BOUND('',#722,.T.);
#490=FACE_OUTER_BOUND('',#723,.T.);
#491=FACE_OUTER_BOUND('',#724,.T.);
#492=FACE_OUTER_BOUND('',#725,.T.);
#493=FACE_OUTER_BOUND('',#726,.T.);
#494=FACE_OUTER_BOUND('',#727,.T.);
#495=FACE_OUTER_BOUND('',#728,.T.);
#496=FACE_OUTER_BOUND('',#729,.T.);
#497=FACE_OUTER_BOUND('',#730,.T.);
#498=FACE_OUTER_BOUND('',#731,.T.);
#499=FACE_OUTER_BOUND('',#732,.T.);
#500=FACE_OUTER_BOUND('',#733,.T.);
#501=FACE_OUTER_BOUND('',#734,.T.);
#502=FACE_OUTER_BOUND('',#735,.T.);
#503=FACE_OUTER_BOUND('',#736,.T.);
#504=FACE_OUTER_BOUND('',#737,.T.);
#505=FACE_OUTER_BOUND('',#738,.T.);
#506=FACE_OUTER_BOUND('',#739,.T.);
#507=FACE_OUTER_BOUND('',#740,.T.);
#508=FACE_OUTER_BOUND('',#741,.T.);
#509=FACE_OUTER_BOUND('',#742,.T.);
#510=FACE_OUTER_BOUND('',#743,.T.);
#511=FACE_OUTER_BOUND('',#744,.T.);
#512=FACE_OUTER_BOUND('',#745,.T.);
#513=FACE_OUTER_BOUND('',#746,.T.);
#514=FACE_OUTER_BOUND('',#747,.T.);
#515=FACE_OUTER_BOUND('',#748,.T.);
#516=FACE_OUTER_BOUND('',#749,.T.);
#517=FACE_OUTER_BOUND('',#750,.T.);
#518=FACE_OUTER_BOUND('',#751,.T.);
#519=FACE_OUTER_BOUND('',#761,.T.);
#520=FACE_OUTER_BOUND('',#771,.T.);
#521=FACE_OUTER_BOUND('',#772,.T.);
#522=FACE_OUTER_BOUND('',#773,.T.);
#523=FACE_OUTER_BOUND('',#774,.T.);
#524=FACE_OUTER_BOUND('',#775,.T.);
#525=FACE_OUTER_BOUND('',#776,.T.);
#526=FACE_OUTER_BOUND('',#777,.T.);
#527=FACE_OUTER_BOUND('',#778,.T.);
#528=FACE_OUTER_BOUND('',#779,.T.);
#529=FACE_OUTER_BOUND('',#780,.T.);
#530=FACE_OUTER_BOUND('',#781,.T.);
#531=FACE_OUTER_BOUND('',#782,.T.);
#532=FACE_OUTER_BOUND('',#783,.T.);
#533=FACE_OUTER_BOUND('',#784,.T.);
#534=FACE_OUTER_BOUND('',#785,.T.);
#535=FACE_OUTER_BOUND('',#786,.T.);
#536=FACE_OUTER_BOUND('',#787,.T.);
#537=FACE_OUTER_BOUND('',#788,.T.);
#538=FACE_OUTER_BOUND('',#789,.T.);
#539=FACE_OUTER_BOUND('',#790,.T.);
#540=FACE_OUTER_BOUND('',#791,.T.);
#541=FACE_OUTER_BOUND('',#792,.T.);
#542=FACE_OUTER_BOUND('',#793,.T.);
#543=FACE_OUTER_BOUND('',#794,.T.);
#544=FACE_OUTER_BOUND('',#795,.T.);
#545=FACE_OUTER_BOUND('',#796,.T.);
#546=FACE_OUTER_BOUND('',#798,.T.);
#547=FACE_OUTER_BOUND('',#799,.T.);
#548=FACE_OUTER_BOUND('',#800,.T.);
#549=FACE_OUTER_BOUND('',#801,.T.);
#550=FACE_OUTER_BOUND('',#802,.T.);
#551=FACE_OUTER_BOUND('',#803,.T.);
#552=FACE_OUTER_BOUND('',#804,.T.);
#553=FACE_OUTER_BOUND('',#805,.T.);
#554=FACE_OUTER_BOUND('',#806,.T.);
#555=FACE_OUTER_BOUND('',#807,.T.);
#556=FACE_OUTER_BOUND('',#808,.T.);
#557=FACE_OUTER_BOUND('',#809,.T.);
#558=FACE_OUTER_BOUND('',#810,.T.);
#559=FACE_OUTER_BOUND('',#811,.T.);
#560=FACE_OUTER_BOUND('',#812,.T.);
#561=FACE_OUTER_BOUND('',#814,.T.);
#562=FACE_OUTER_BOUND('',#815,.T.);
#563=FACE_OUTER_BOUND('',#816,.T.);
#564=FACE_OUTER_BOUND('',#817,.T.);
#565=FACE_OUTER_BOUND('',#819,.T.);
#566=FACE_OUTER_BOUND('',#820,.T.);
#567=FACE_OUTER_BOUND('',#821,.T.);
#568=FACE_OUTER_BOUND('',#822,.T.);
#569=FACE_OUTER_BOUND('',#824,.T.);
#570=FACE_OUTER_BOUND('',#825,.T.);
#571=FACE_OUTER_BOUND('',#826,.T.);
#572=FACE_OUTER_BOUND('',#827,.T.);
#573=FACE_OUTER_BOUND('',#829,.T.);
#574=FACE_OUTER_BOUND('',#830,.T.);
#575=FACE_OUTER_BOUND('',#831,.T.);
#576=FACE_OUTER_BOUND('',#832,.T.);
#577=FACE_OUTER_BOUND('',#833,.T.);
#578=FACE_OUTER_BOUND('',#834,.T.);
#579=FACE_OUTER_BOUND('',#835,.T.);
#580=FACE_OUTER_BOUND('',#836,.T.);
#581=FACE_OUTER_BOUND('',#837,.T.);
#582=FACE_OUTER_BOUND('',#838,.T.);
#583=FACE_OUTER_BOUND('',#840,.T.);
#584=FACE_OUTER_BOUND('',#842,.T.);
#585=FACE_OUTER_BOUND('',#850,.T.);
#586=FACE_OUTER_BOUND('',#858,.T.);
#587=FACE_OUTER_BOUND('',#859,.T.);
#588=FACE_OUTER_BOUND('',#860,.T.);
#589=FACE_OUTER_BOUND('',#861,.T.);
#590=FACE_OUTER_BOUND('',#863,.T.);
#591=FACE_OUTER_BOUND('',#865,.T.);
#592=FACE_OUTER_BOUND('',#866,.T.);
#593=FACE_OUTER_BOUND('',#867,.T.);
#594=FACE_OUTER_BOUND('',#868,.T.);
#595=FACE_OUTER_BOUND('',#869,.T.);
#596=FACE_OUTER_BOUND('',#870,.T.);
#597=FACE_OUTER_BOUND('',#871,.T.);
#598=FACE_OUTER_BOUND('',#872,.T.);
#599=FACE_OUTER_BOUND('',#873,.T.);
#600=FACE_OUTER_BOUND('',#874,.T.);
#601=FACE_OUTER_BOUND('',#875,.T.);
#602=FACE_OUTER_BOUND('',#876,.T.);
#603=FACE_OUTER_BOUND('',#877,.T.);
#604=FACE_OUTER_BOUND('',#878,.T.);
#605=FACE_OUTER_BOUND('',#879,.T.);
#606=FACE_OUTER_BOUND('',#880,.T.);
#607=FACE_OUTER_BOUND('',#881,.T.);
#608=FACE_OUTER_BOUND('',#882,.T.);
#609=FACE_OUTER_BOUND('',#883,.T.);
#610=FACE_OUTER_BOUND('',#884,.T.);
#611=EDGE_LOOP('',(#2533,#2534,#2535,#2536,#2537,#2538,#2539,#2540,#2541,
#2542,#2543,#2544));
#612=EDGE_LOOP('',(#2545));
#613=EDGE_LOOP('',(#2546));
#614=EDGE_LOOP('',(#2547));
#615=EDGE_LOOP('',(#2548));
#616=EDGE_LOOP('',(#2549,#2550,#2551,#2552));
#617=EDGE_LOOP('',(#2553,#2554,#2555,#2556));
#618=EDGE_LOOP('',(#2557,#2558,#2559,#2560,#2561,#2562,#2563,#2564));
#619=EDGE_LOOP('',(#2565,#2566,#2567,#2568,#2569,#2570,#2571,#2572,#2573,
#2574,#2575,#2576));
#620=EDGE_LOOP('',(#2577,#2578,#2579,#2580,#2581,#2582,#2583,#2584));
#621=EDGE_LOOP('',(#2585,#2586,#2587,#2588,#2589,#2590));
#622=EDGE_LOOP('',(#2591,#2592,#2593,#2594,#2595,#2596));
#623=EDGE_LOOP('',(#2597,#2598,#2599,#2600,#2601,#2602,#2603,#2604,#2605,
#2606,#2607,#2608));
#624=EDGE_LOOP('',(#2609,#2610,#2611,#2612));
#625=EDGE_LOOP('',(#2613));
#626=EDGE_LOOP('',(#2614));
#627=EDGE_LOOP('',(#2615));
#628=EDGE_LOOP('',(#2616));
#629=EDGE_LOOP('',(#2617,#2618,#2619,#2620));
#630=EDGE_LOOP('',(#2621,#2622,#2623,#2624));
#631=EDGE_LOOP('',(#2625,#2626,#2627,#2628));
#632=EDGE_LOOP('',(#2629,#2630,#2631,#2632,#2633,#2634));
#633=EDGE_LOOP('',(#2635,#2636,#2637,#2638,#2639,#2640));
#634=EDGE_LOOP('',(#2641,#2642,#2643,#2644));
#635=EDGE_LOOP('',(#2645));
#636=EDGE_LOOP('',(#2646));
#637=EDGE_LOOP('',(#2647,#2648,#2649,#2650,#2651,#2652,#2653,#2654));
#638=EDGE_LOOP('',(#2655,#2656,#2657,#2658,#2659,#2660,#2661,#2662,#2663,
#2664,#2665,#2666));
#639=EDGE_LOOP('',(#2667,#2668,#2669,#2670,#2671,#2672,#2673,#2674));
#640=EDGE_LOOP('',(#2675,#2676,#2677,#2678));
#641=EDGE_LOOP('',(#2679));
#642=EDGE_LOOP('',(#2680));
#643=EDGE_LOOP('',(#2681,#2682,#2683,#2684,#2685,#2686,#2687,#2688));
#644=EDGE_LOOP('',(#2689,#2690,#2691,#2692,#2693));
#645=EDGE_LOOP('',(#2694,#2695,#2696,#2697,#2698,#2699,#2700,#2701,#2702));
#646=EDGE_LOOP('',(#2703,#2704,#2705,#2706,#2707,#2708,#2709,#2710,#2711));
#647=EDGE_LOOP('',(#2712,#2713,#2714,#2715,#2716));
#648=EDGE_LOOP('',(#2717,#2718,#2719,#2720,#2721,#2722,#2723,#2724));
#649=EDGE_LOOP('',(#2725,#2726,#2727,#2728,#2729,#2730,#2731,#2732));
#650=EDGE_LOOP('',(#2733,#2734,#2735,#2736,#2737));
#651=EDGE_LOOP('',(#2738,#2739,#2740,#2741,#2742,#2743,#2744,#2745,#2746));
#652=EDGE_LOOP('',(#2747,#2748,#2749,#2750,#2751,#2752,#2753,#2754));
#653=EDGE_LOOP('',(#2755,#2756,#2757,#2758,#2759,#2760,#2761,#2762,#2763));
#654=EDGE_LOOP('',(#2764,#2765,#2766,#2767,#2768));
#655=EDGE_LOOP('',(#2769,#2770,#2771,#2772));
#656=EDGE_LOOP('',(#2773,#2774,#2775,#2776));
#657=EDGE_LOOP('',(#2777,#2778,#2779,#2780));
#658=EDGE_LOOP('',(#2781,#2782,#2783,#2784));
#659=EDGE_LOOP('',(#2785,#2786,#2787,#2788));
#660=EDGE_LOOP('',(#2789,#2790,#2791,#2792));
#661=EDGE_LOOP('',(#2793,#2794,#2795,#2796));
#662=EDGE_LOOP('',(#2797,#2798,#2799,#2800));
#663=EDGE_LOOP('',(#2801,#2802,#2803,#2804));
#664=EDGE_LOOP('',(#2805,#2806,#2807,#2808));
#665=EDGE_LOOP('',(#2809,#2810,#2811,#2812));
#666=EDGE_LOOP('',(#2813,#2814,#2815,#2816));
#667=EDGE_LOOP('',(#2817,#2818,#2819,#2820,#2821,#2822,#2823,#2824,#2825));
#668=EDGE_LOOP('',(#2826,#2827,#2828,#2829,#2830,#2831));
#669=EDGE_LOOP('',(#2832,#2833,#2834,#2835,#2836,#2837,#2838,#2839,#2840));
#670=EDGE_LOOP('',(#2841,#2842,#2843,#2844,#2845,#2846,#2847,#2848,#2849));
#671=EDGE_LOOP('',(#2850,#2851,#2852,#2853,#2854,#2855));
#672=EDGE_LOOP('',(#2856,#2857,#2858,#2859,#2860,#2861,#2862,#2863,#2864));
#673=EDGE_LOOP('',(#2865,#2866,#2867,#2868));
#674=EDGE_LOOP('',(#2869,#2870,#2871,#2872));
#675=EDGE_LOOP('',(#2873,#2874,#2875,#2876));
#676=EDGE_LOOP('',(#2877,#2878,#2879,#2880));
#677=EDGE_LOOP('',(#2881,#2882,#2883,#2884,#2885,#2886));
#678=EDGE_LOOP('',(#2887,#2888,#2889,#2890,#2891,#2892));
#679=EDGE_LOOP('',(#2893,#2894,#2895,#2896));
#680=EDGE_LOOP('',(#2897,#2898,#2899,#2900));
#681=EDGE_LOOP('',(#2901,#2902,#2903,#2904));
#682=EDGE_LOOP('',(#2905,#2906,#2907,#2908));
#683=EDGE_LOOP('',(#2909,#2910,#2911,#2912,#2913,#2914));
#684=EDGE_LOOP('',(#2915,#2916,#2917,#2918,#2919,#2920));
#685=EDGE_LOOP('',(#2921,#2922,#2923,#2924));
#686=EDGE_LOOP('',(#2925,#2926,#2927,#2928));
#687=EDGE_LOOP('',(#2929,#2930,#2931,#2932));
#688=EDGE_LOOP('',(#2933,#2934,#2935,#2936));
#689=EDGE_LOOP('',(#2937,#2938,#2939,#2940,#2941,#2942));
#690=EDGE_LOOP('',(#2943,#2944,#2945,#2946,#2947,#2948));
#691=EDGE_LOOP('',(#2949,#2950,#2951,#2952));
#692=EDGE_LOOP('',(#2953,#2954,#2955,#2956));
#693=EDGE_LOOP('',(#2957,#2958,#2959,#2960));
#694=EDGE_LOOP('',(#2961,#2962,#2963,#2964));
#695=EDGE_LOOP('',(#2965,#2966,#2967,#2968,#2969,#2970));
#696=EDGE_LOOP('',(#2971,#2972,#2973,#2974,#2975,#2976));
#697=EDGE_LOOP('',(#2977,#2978,#2979,#2980));
#698=EDGE_LOOP('',(#2981,#2982,#2983,#2984));
#699=EDGE_LOOP('',(#2985,#2986,#2987,#2988));
#700=EDGE_LOOP('',(#2989,#2990,#2991,#2992));
#701=EDGE_LOOP('',(#2993,#2994,#2995,#2996));
#702=EDGE_LOOP('',(#2997,#2998,#2999,#3000));
#703=EDGE_LOOP('',(#3001,#3002,#3003,#3004));
#704=EDGE_LOOP('',(#3005,#3006,#3007,#3008));
#705=EDGE_LOOP('',(#3009,#3010,#3011,#3012));
#706=EDGE_LOOP('',(#3013,#3014,#3015,#3016));
#707=EDGE_LOOP('',(#3017,#3018,#3019,#3020));
#708=EDGE_LOOP('',(#3021,#3022,#3023,#3024));
#709=EDGE_LOOP('',(#3025,#3026,#3027,#3028));
#710=EDGE_LOOP('',(#3029,#3030,#3031,#3032));
#711=EDGE_LOOP('',(#3033,#3034,#3035,#3036));
#712=EDGE_LOOP('',(#3037,#3038,#3039,#3040));
#713=EDGE_LOOP('',(#3041,#3042,#3043,#3044));
#714=EDGE_LOOP('',(#3045,#3046,#3047,#3048));
#715=EDGE_LOOP('',(#3049,#3050,#3051,#3052));
#716=EDGE_LOOP('',(#3053,#3054,#3055,#3056));
#717=EDGE_LOOP('',(#3057,#3058,#3059,#3060));
#718=EDGE_LOOP('',(#3061,#3062,#3063,#3064));
#719=EDGE_LOOP('',(#3065,#3066,#3067,#3068));
#720=EDGE_LOOP('',(#3069,#3070,#3071,#3072));
#721=EDGE_LOOP('',(#3073,#3074,#3075,#3076));
#722=EDGE_LOOP('',(#3077,#3078,#3079,#3080));
#723=EDGE_LOOP('',(#3081,#3082,#3083,#3084));
#724=EDGE_LOOP('',(#3085,#3086,#3087,#3088));
#725=EDGE_LOOP('',(#3089,#3090,#3091,#3092));
#726=EDGE_LOOP('',(#3093,#3094,#3095,#3096));
#727=EDGE_LOOP('',(#3097,#3098,#3099,#3100));
#728=EDGE_LOOP('',(#3101,#3102,#3103,#3104));
#729=EDGE_LOOP('',(#3105,#3106,#3107,#3108));
#730=EDGE_LOOP('',(#3109,#3110,#3111,#3112));
#731=EDGE_LOOP('',(#3113,#3114,#3115,#3116));
#732=EDGE_LOOP('',(#3117,#3118,#3119,#3120));
#733=EDGE_LOOP('',(#3121,#3122,#3123,#3124));
#734=EDGE_LOOP('',(#3125,#3126,#3127,#3128));
#735=EDGE_LOOP('',(#3129,#3130,#3131,#3132));
#736=EDGE_LOOP('',(#3133,#3134,#3135,#3136));
#737=EDGE_LOOP('',(#3137,#3138,#3139,#3140));
#738=EDGE_LOOP('',(#3141,#3142,#3143,#3144));
#739=EDGE_LOOP('',(#3145,#3146,#3147,#3148));
#740=EDGE_LOOP('',(#3149,#3150,#3151,#3152));
#741=EDGE_LOOP('',(#3153,#3154,#3155,#3156));
#742=EDGE_LOOP('',(#3157,#3158,#3159,#3160));
#743=EDGE_LOOP('',(#3161,#3162,#3163,#3164));
#744=EDGE_LOOP('',(#3165,#3166,#3167,#3168));
#745=EDGE_LOOP('',(#3169,#3170,#3171,#3172));
#746=EDGE_LOOP('',(#3173,#3174,#3175,#3176));
#747=EDGE_LOOP('',(#3177,#3178,#3179,#3180));
#748=EDGE_LOOP('',(#3181,#3182,#3183,#3184));
#749=EDGE_LOOP('',(#3185,#3186,#3187,#3188));
#750=EDGE_LOOP('',(#3189,#3190,#3191,#3192));
#751=EDGE_LOOP('',(#3193,#3194,#3195,#3196));
#752=EDGE_LOOP('',(#3197,#3198,#3199,#3200));
#753=EDGE_LOOP('',(#3201,#3202,#3203,#3204));
#754=EDGE_LOOP('',(#3205,#3206,#3207,#3208));
#755=EDGE_LOOP('',(#3209,#3210,#3211,#3212));
#756=EDGE_LOOP('',(#3213,#3214,#3215,#3216));
#757=EDGE_LOOP('',(#3217));
#758=EDGE_LOOP('',(#3218));
#759=EDGE_LOOP('',(#3219));
#760=EDGE_LOOP('',(#3220));
#761=EDGE_LOOP('',(#3221,#3222,#3223,#3224));
#762=EDGE_LOOP('',(#3225,#3226,#3227,#3228));
#763=EDGE_LOOP('',(#3229,#3230,#3231,#3232));
#764=EDGE_LOOP('',(#3233,#3234,#3235,#3236));
#765=EDGE_LOOP('',(#3237,#3238,#3239,#3240));
#766=EDGE_LOOP('',(#3241,#3242,#3243,#3244));
#767=EDGE_LOOP('',(#3245));
#768=EDGE_LOOP('',(#3246));
#769=EDGE_LOOP('',(#3247));
#770=EDGE_LOOP('',(#3248));
#771=EDGE_LOOP('',(#3249,#3250,#3251,#3252));
#772=EDGE_LOOP('',(#3253,#3254,#3255,#3256));
#773=EDGE_LOOP('',(#3257,#3258,#3259,#3260));
#774=EDGE_LOOP('',(#3261,#3262,#3263,#3264));
#775=EDGE_LOOP('',(#3265,#3266,#3267,#3268));
#776=EDGE_LOOP('',(#3269,#3270,#3271,#3272));
#777=EDGE_LOOP('',(#3273,#3274,#3275,#3276));
#778=EDGE_LOOP('',(#3277,#3278,#3279,#3280));
#779=EDGE_LOOP('',(#3281,#3282,#3283,#3284));
#780=EDGE_LOOP('',(#3285,#3286,#3287,#3288));
#781=EDGE_LOOP('',(#3289,#3290,#3291,#3292));
#782=EDGE_LOOP('',(#3293,#3294,#3295,#3296));
#783=EDGE_LOOP('',(#3297,#3298,#3299,#3300));
#784=EDGE_LOOP('',(#3301,#3302,#3303,#3304));
#785=EDGE_LOOP('',(#3305,#3306,#3307,#3308));
#786=EDGE_LOOP('',(#3309,#3310,#3311,#3312));
#787=EDGE_LOOP('',(#3313,#3314,#3315,#3316));
#788=EDGE_LOOP('',(#3317,#3318,#3319,#3320));
#789=EDGE_LOOP('',(#3321,#3322,#3323,#3324));
#790=EDGE_LOOP('',(#3325,#3326,#3327,#3328));
#791=EDGE_LOOP('',(#3329,#3330,#3331,#3332));
#792=EDGE_LOOP('',(#3333,#3334,#3335,#3336));
#793=EDGE_LOOP('',(#3337,#3338,#3339,#3340));
#794=EDGE_LOOP('',(#3341,#3342,#3343,#3344));
#795=EDGE_LOOP('',(#3345,#3346,#3347,#3348,#3349,#3350,#3351,#3352,#3353,
#3354,#3355,#3356));
#796=EDGE_LOOP('',(#3357,#3358,#3359,#3360,#3361,#3362,#3363,#3364));
#797=EDGE_LOOP('',(#3365));
#798=EDGE_LOOP('',(#3366));
#799=EDGE_LOOP('',(#3367,#3368,#3369,#3370,#3371));
#800=EDGE_LOOP('',(#3372,#3373,#3374,#3375));
#801=EDGE_LOOP('',(#3376,#3377,#3378,#3379));
#802=EDGE_LOOP('',(#3380,#3381,#3382,#3383));
#803=EDGE_LOOP('',(#3384,#3385,#3386,#3387));
#804=EDGE_LOOP('',(#3388,#3389,#3390,#3391));
#805=EDGE_LOOP('',(#3392,#3393,#3394,#3395));
#806=EDGE_LOOP('',(#3396,#3397,#3398,#3399));
#807=EDGE_LOOP('',(#3400,#3401,#3402,#3403));
#808=EDGE_LOOP('',(#3404));
#809=EDGE_LOOP('',(#3405,#3406,#3407,#3408,#3409,#3410));
#810=EDGE_LOOP('',(#3411,#3412,#3413,#3414,#3415));
#811=EDGE_LOOP('',(#3416,#3417,#3418,#3419,#3420));
#812=EDGE_LOOP('',(#3421));
#813=EDGE_LOOP('',(#3422));
#814=EDGE_LOOP('',(#3423,#3424,#3425,#3426));
#815=EDGE_LOOP('',(#3427,#3428,#3429,#3430));
#816=EDGE_LOOP('',(#3431,#3432,#3433,#3434));
#817=EDGE_LOOP('',(#3435));
#818=EDGE_LOOP('',(#3436));
#819=EDGE_LOOP('',(#3437,#3438,#3439,#3440,#3441,#3442));
#820=EDGE_LOOP('',(#3443,#3444,#3445,#3446,#3447));
#821=EDGE_LOOP('',(#3448,#3449,#3450,#3451,#3452));
#822=EDGE_LOOP('',(#3453));
#823=EDGE_LOOP('',(#3454));
#824=EDGE_LOOP('',(#3455,#3456,#3457,#3458));
#825=EDGE_LOOP('',(#3459,#3460,#3461,#3462));
#826=EDGE_LOOP('',(#3463,#3464,#3465,#3466));
#827=EDGE_LOOP('',(#3467));
#828=EDGE_LOOP('',(#3468));
#829=EDGE_LOOP('',(#3469,#3470,#3471,#3472));
#830=EDGE_LOOP('',(#3473,#3474,#3475,#3476,#3477));
#831=EDGE_LOOP('',(#3478,#3479,#3480,#3481));
#832=EDGE_LOOP('',(#3482,#3483,#3484,#3485));
#833=EDGE_LOOP('',(#3486,#3487,#3488,#3489));
#834=EDGE_LOOP('',(#3490,#3491,#3492,#3493));
#835=EDGE_LOOP('',(#3494,#3495,#3496,#3497));
#836=EDGE_LOOP('',(#3498,#3499,#3500,#3501));
#837=EDGE_LOOP('',(#3502,#3503,#3504,#3505));
#838=EDGE_LOOP('',(#3506));
#839=EDGE_LOOP('',(#3507));
#840=EDGE_LOOP('',(#3508));
#841=EDGE_LOOP('',(#3509));
#842=EDGE_LOOP('',(#3510));
#843=EDGE_LOOP('',(#3511));
#844=EDGE_LOOP('',(#3512));
#845=EDGE_LOOP('',(#3513));
#846=EDGE_LOOP('',(#3514));
#847=EDGE_LOOP('',(#3515));
#848=EDGE_LOOP('',(#3516));
#849=EDGE_LOOP('',(#3517));
#850=EDGE_LOOP('',(#3518));
#851=EDGE_LOOP('',(#3519));
#852=EDGE_LOOP('',(#3520));
#853=EDGE_LOOP('',(#3521));
#854=EDGE_LOOP('',(#3522));
#855=EDGE_LOOP('',(#3523));
#856=EDGE_LOOP('',(#3524));
#857=EDGE_LOOP('',(#3525));
#858=EDGE_LOOP('',(#3526,#3527,#3528,#3529));
#859=EDGE_LOOP('',(#3530,#3531,#3532,#3533));
#860=EDGE_LOOP('',(#3534,#3535,#3536,#3537));
#861=EDGE_LOOP('',(#3538));
#862=EDGE_LOOP('',(#3539));
#863=EDGE_LOOP('',(#3540));
#864=EDGE_LOOP('',(#3541));
#865=EDGE_LOOP('',(#3542,#3543,#3544,#3545));
#866=EDGE_LOOP('',(#3546,#3547,#3548,#3549,#3550));
#867=EDGE_LOOP('',(#3551,#3552,#3553,#3554,#3555));
#868=EDGE_LOOP('',(#3556,#3557,#3558,#3559,#3560));
#869=EDGE_LOOP('',(#3561,#3562,#3563,#3564));
#870=EDGE_LOOP('',(#3565,#3566,#3567,#3568));
#871=EDGE_LOOP('',(#3569,#3570,#3571,#3572));
#872=EDGE_LOOP('',(#3573,#3574,#3575,#3576));
#873=EDGE_LOOP('',(#3577,#3578,#3579,#3580));
#874=EDGE_LOOP('',(#3581,#3582,#3583,#3584));
#875=EDGE_LOOP('',(#3585,#3586,#3587,#3588));
#876=EDGE_LOOP('',(#3589,#3590,#3591,#3592));
#877=EDGE_LOOP('',(#3593,#3594,#3595,#3596));
#878=EDGE_LOOP('',(#3597,#3598,#3599,#3600));
#879=EDGE_LOOP('',(#3601,#3602,#3603,#3604));
#880=EDGE_LOOP('',(#3605,#3606,#3607,#3608));
#881=EDGE_LOOP('',(#3609,#3610,#3611,#3612));
#882=EDGE_LOOP('',(#3613,#3614,#3615,#3616));
#883=EDGE_LOOP('',(#3617,#3618,#3619,#3620));
#884=EDGE_LOOP('',(#3621,#3622,#3623,#3624));
#885=LINE('',#5612,#1263);
#886=LINE('',#5614,#1264);
#887=LINE('',#5616,#1265);
#888=LINE('',#5618,#1266);
#889=LINE('',#5620,#1267);
#890=LINE('',#5622,#1268);
#891=LINE('',#5624,#1269);
#892=LINE('',#5626,#1270);
#893=LINE('',#5628,#1271);
#894=LINE('',#5630,#1272);
#895=LINE('',#5632,#1273);
#896=LINE('',#5633,#1274);
#897=LINE('',#5644,#1275);
#898=LINE('',#5646,#1276);
#899=LINE('',#5648,#1277);
#900=LINE('',#5649,#1278);
#901=LINE('',#5652,#1279);
#902=LINE('',#5654,#1280);
#903=LINE('',#5656,#1281);
#904=LINE('',#5657,#1282);
#905=LINE('',#5661,#1283);
#906=LINE('',#5663,#1284);
#907=LINE('',#5665,#1285);
#908=LINE('',#5666,#1286);
#909=LINE('',#5668,#1287);
#910=LINE('',#5670,#1288);
#911=LINE('',#5671,#1289);
#912=LINE('',#5675,#1290);
#913=LINE('',#5677,#1291);
#914=LINE('',#5678,#1292);
#915=LINE('',#5680,#1293);
#916=LINE('',#5682,#1294);
#917=LINE('',#5684,#1295);
#918=LINE('',#5686,#1296);
#919=LINE('',#5688,#1297);
#920=LINE('',#5690,#1298);
#921=LINE('',#5692,#1299);
#922=LINE('',#5693,#1300);
#923=LINE('',#5697,#1301);
#924=LINE('',#5699,#1302);
#925=LINE('',#5700,#1303);
#926=LINE('',#5701,#1304);
#927=LINE('',#5703,#1305);
#928=LINE('',#5704,#1306);
#929=LINE('',#5708,#1307);
#930=LINE('',#5710,#1308);
#931=LINE('',#5712,#1309);
#932=LINE('',#5714,#1310);
#933=LINE('',#5716,#1311);
#934=LINE('',#5717,#1312);
#935=LINE('',#5721,#1313);
#936=LINE('',#5723,#1314);
#937=LINE('',#5725,#1315);
#938=LINE('',#5727,#1316);
#939=LINE('',#5729,#1317);
#940=LINE('',#5730,#1318);
#941=LINE('',#5734,#1319);
#942=LINE('',#5736,#1320);
#943=LINE('',#5738,#1321);
#944=LINE('',#5740,#1322);
#945=LINE('',#5742,#1323);
#946=LINE('',#5744,#1324);
#947=LINE('',#5746,#1325);
#948=LINE('',#5748,#1326);
#949=LINE('',#5750,#1327);
#950=LINE('',#5752,#1328);
#951=LINE('',#5754,#1329);
#952=LINE('',#5755,#1330);
#953=LINE('',#5758,#1331);
#954=LINE('',#5760,#1332);
#955=LINE('',#5762,#1333);
#956=LINE('',#5763,#1334);
#957=LINE('',#5774,#1335);
#958=LINE('',#5776,#1336);
#959=LINE('',#5778,#1337);
#960=LINE('',#5779,#1338);
#961=LINE('',#5783,#1339);
#962=LINE('',#5785,#1340);
#963=LINE('',#5787,#1341);
#964=LINE('',#5788,#1342);
#965=LINE('',#5791,#1343);
#966=LINE('',#5793,#1344);
#967=LINE('',#5794,#1345);
#968=LINE('',#5798,#1346);
#969=LINE('',#5799,#1347);
#970=LINE('',#5801,#1348);
#971=LINE('',#5803,#1349);
#972=LINE('',#5804,#1350);
#973=LINE('',#5808,#1351);
#974=LINE('',#5810,#1352);
#975=LINE('',#5812,#1353);
#976=LINE('',#5813,#1354);
#977=LINE('',#5814,#1355);
#978=LINE('',#5822,#1356);
#979=LINE('',#5824,#1357);
#980=LINE('',#5825,#1358);
#981=LINE('',#5827,#1359);
#982=LINE('',#5828,#1360);
#983=LINE('',#5831,#1361);
#984=LINE('',#5833,#1362);
#985=LINE('',#5834,#1363);
#986=LINE('',#5836,#1364);
#987=LINE('',#5837,#1365);
#988=LINE('',#5839,#1366);
#989=LINE('',#5841,#1367);
#990=LINE('',#5842,#1368);
#991=LINE('',#5845,#1369);
#992=LINE('',#5847,#1370);
#993=LINE('',#5848,#1371);
#994=LINE('',#5849,#1372);
#995=LINE('',#5857,#1373);
#996=LINE('',#5859,#1374);
#997=LINE('',#5861,#1375);
#998=LINE('',#5862,#1376);
#999=LINE('',#5863,#1377);
#1000=LINE('',#5867,#1378);
#1001=LINE('',#5870,#1379);
#1002=LINE('',#5874,#1380);
#1003=LINE('',#5876,#1381);
#1004=LINE('',#5878,#1382);
#1005=LINE('',#5879,#1383);
#1006=LINE('',#5885,#1384);
#1007=LINE('',#5886,#1385);
#1008=LINE('',#5888,#1386);
#1009=LINE('',#5890,#1387);
#1010=LINE('',#5892,#1388);
#1011=LINE('',#5893,#1389);
#1012=LINE('',#5895,#1390);
#1013=LINE('',#5899,#1391);
#1014=LINE('',#5901,#1392);
#1015=LINE('',#5903,#1393);
#1016=LINE('',#5904,#1394);
#1017=LINE('',#5906,#1395);
#1018=LINE('',#5908,#1396);
#1019=LINE('',#5910,#1397);
#1020=LINE('',#5912,#1398);
#1021=LINE('',#5913,#1399);
#1022=LINE('',#5916,#1400);
#1023=LINE('',#5922,#1401);
#1024=LINE('',#5924,#1402);
#1025=LINE('',#5926,#1403);
#1026=LINE('',#5928,#1404);
#1027=LINE('',#5929,#1405);
#1028=LINE('',#5932,#1406);
#1029=LINE('',#5934,#1407);
#1030=LINE('',#5936,#1408);
#1031=LINE('',#5937,#1409);
#1032=LINE('',#5938,#1410);
#1033=LINE('',#5941,#1411);
#1034=LINE('',#5943,#1412);
#1035=LINE('',#5947,#1413);
#1036=LINE('',#5949,#1414);
#1037=LINE('',#5951,#1415);
#1038=LINE('',#5952,#1416);
#1039=LINE('',#5956,#1417);
#1040=LINE('',#5957,#1418);
#1041=LINE('',#5959,#1419);
#1042=LINE('',#5961,#1420);
#1043=LINE('',#5964,#1421);
#1044=LINE('',#5965,#1422);
#1045=LINE('',#5967,#1423);
#1046=LINE('',#5969,#1424);
#1047=LINE('',#5972,#1425);
#1048=LINE('',#5974,#1426);
#1049=LINE('',#5976,#1427);
#1050=LINE('',#5978,#1428);
#1051=LINE('',#5981,#1429);
#1052=LINE('',#5983,#1430);
#1053=LINE('',#5987,#1431);
#1054=LINE('',#5989,#1432);
#1055=LINE('',#5991,#1433);
#1056=LINE('',#5992,#1434);
#1057=LINE('',#5995,#1435);
#1058=LINE('',#6002,#1436);
#1059=LINE('',#6004,#1437);
#1060=LINE('',#6006,#1438);
#1061=LINE('',#6008,#1439);
#1062=LINE('',#6009,#1440);
#1063=LINE('',#6012,#1441);
#1064=LINE('',#6014,#1442);
#1065=LINE('',#6018,#1443);
#1066=LINE('',#6020,#1444);
#1067=LINE('',#6022,#1445);
#1068=LINE('',#6023,#1446);
#1069=LINE('',#6026,#1447);
#1070=LINE('',#6033,#1448);
#1071=LINE('',#6035,#1449);
#1072=LINE('',#6037,#1450);
#1073=LINE('',#6039,#1451);
#1074=LINE('',#6040,#1452);
#1075=LINE('',#6043,#1453);
#1076=LINE('',#6045,#1454);
#1077=LINE('',#6046,#1455);
#1078=LINE('',#6049,#1456);
#1079=LINE('',#6050,#1457);
#1080=LINE('',#6052,#1458);
#1081=LINE('',#6054,#1459);
#1082=LINE('',#6055,#1460);
#1083=LINE('',#6059,#1461);
#1084=LINE('',#6061,#1462);
#1085=LINE('',#6063,#1463);
#1086=LINE('',#6065,#1464);
#1087=LINE('',#6067,#1465);
#1088=LINE('',#6068,#1466);
#1089=LINE('',#6072,#1467);
#1090=LINE('',#6073,#1468);
#1091=LINE('',#6077,#1469);
#1092=LINE('',#6078,#1470);
#1093=LINE('',#6079,#1471);
#1094=LINE('',#6081,#1472);
#1095=LINE('',#6082,#1473);
#1096=LINE('',#6084,#1474);
#1097=LINE('',#6088,#1475);
#1098=LINE('',#6090,#1476);
#1099=LINE('',#6092,#1477);
#1100=LINE('',#6094,#1478);
#1101=LINE('',#6096,#1479);
#1102=LINE('',#6097,#1480);
#1103=LINE('',#6101,#1481);
#1104=LINE('',#6102,#1482);
#1105=LINE('',#6106,#1483);
#1106=LINE('',#6107,#1484);
#1107=LINE('',#6108,#1485);
#1108=LINE('',#6110,#1486);
#1109=LINE('',#6111,#1487);
#1110=LINE('',#6113,#1488);
#1111=LINE('',#6117,#1489);
#1112=LINE('',#6119,#1490);
#1113=LINE('',#6121,#1491);
#1114=LINE('',#6123,#1492);
#1115=LINE('',#6125,#1493);
#1116=LINE('',#6126,#1494);
#1117=LINE('',#6130,#1495);
#1118=LINE('',#6131,#1496);
#1119=LINE('',#6135,#1497);
#1120=LINE('',#6136,#1498);
#1121=LINE('',#6137,#1499);
#1122=LINE('',#6139,#1500);
#1123=LINE('',#6140,#1501);
#1124=LINE('',#6142,#1502);
#1125=LINE('',#6146,#1503);
#1126=LINE('',#6148,#1504);
#1127=LINE('',#6150,#1505);
#1128=LINE('',#6152,#1506);
#1129=LINE('',#6154,#1507);
#1130=LINE('',#6155,#1508);
#1131=LINE('',#6158,#1509);
#1132=LINE('',#6160,#1510);
#1133=LINE('',#6161,#1511);
#1134=LINE('',#6165,#1512);
#1135=LINE('',#6166,#1513);
#1136=LINE('',#6168,#1514);
#1137=LINE('',#6252,#1515);
#1138=LINE('',#6254,#1516);
#1139=LINE('',#6259,#1517);
#1140=LINE('',#6261,#1518);
#1141=LINE('',#6263,#1519);
#1142=LINE('',#6264,#1520);
#1143=LINE('',#6267,#1521);
#1144=LINE('',#6269,#1522);
#1145=LINE('',#6270,#1523);
#1146=LINE('',#6273,#1524);
#1147=LINE('',#6275,#1525);
#1148=LINE('',#6276,#1526);
#1149=LINE('',#6278,#1527);
#1150=LINE('',#6279,#1528);
#1151=LINE('',#6285,#1529);
#1152=LINE('',#6288,#1530);
#1153=LINE('',#6293,#1531);
#1154=LINE('',#6296,#1532);
#1155=LINE('',#6301,#1533);
#1156=LINE('',#6304,#1534);
#1157=LINE('',#6309,#1535);
#1158=LINE('',#6312,#1536);
#1159=LINE('',#6317,#1537);
#1160=LINE('',#6320,#1538);
#1161=LINE('',#6332,#1539);
#1162=LINE('',#6336,#1540);
#1163=LINE('',#6340,#1541);
#1164=LINE('',#6344,#1542);
#1165=LINE('',#6348,#1543);
#1166=LINE('',#6352,#1544);
#1167=LINE('',#6356,#1545);
#1168=LINE('',#6360,#1546);
#1169=LINE('',#6364,#1547);
#1170=LINE('',#6368,#1548);
#1171=LINE('',#6379,#1549);
#1172=LINE('',#6381,#1550);
#1173=LINE('',#6383,#1551);
#1174=LINE('',#6385,#1552);
#1175=LINE('',#6387,#1553);
#1176=LINE('',#6388,#1554);
#1177=LINE('',#6390,#1555);
#1178=LINE('',#6392,#1556);
#1179=LINE('',#6395,#1557);
#1180=LINE('',#6396,#1558);
#1181=LINE('',#6398,#1559);
#1182=LINE('',#6400,#1560);
#1183=LINE('',#6403,#1561);
#1184=LINE('',#6404,#1562);
#1185=LINE('',#6406,#1563);
#1186=LINE('',#6408,#1564);
#1187=LINE('',#6411,#1565);
#1188=LINE('',#6412,#1566);
#1189=LINE('',#6414,#1567);
#1190=LINE('',#6416,#1568);
#1191=LINE('',#6419,#1569);
#1192=LINE('',#6420,#1570);
#1193=LINE('',#6422,#1571);
#1194=LINE('',#6424,#1572);
#1195=LINE('',#6434,#1573);
#1196=LINE('',#6438,#1574);
#1197=LINE('',#6442,#1575);
#1198=LINE('',#6446,#1576);
#1199=LINE('',#6450,#1577);
#1200=LINE('',#6454,#1578);
#1201=LINE('',#6456,#1579);
#1202=LINE('',#6457,#1580);
#1203=LINE('',#6459,#1581);
#1204=LINE('',#6461,#1582);
#1205=LINE('',#6462,#1583);
#1206=LINE('',#6469,#1584);
#1207=LINE('',#6470,#1585);
#1208=LINE('',#6471,#1586);
#1209=LINE('',#6473,#1587);
#1210=LINE('',#6475,#1588);
#1211=LINE('',#6479,#1589);
#1212=LINE('',#6481,#1590);
#1213=LINE('',#6482,#1591);
#1214=LINE('',#6484,#1592);
#1215=LINE('',#6486,#1593);
#1216=LINE('',#6491,#1594);
#1217=LINE('',#6507,#1595);
#1218=LINE('',#6514,#1596);
#1219=LINE('',#6526,#1597);
#1220=LINE('',#6540,#1598);
#1221=LINE('',#6545,#1599);
#1222=LINE('',#6555,#1600);
#1223=LINE('',#6567,#1601);
#1224=LINE('',#6575,#1602);
#1225=LINE('',#6581,#1603);
#1226=LINE('',#6587,#1604);
#1227=LINE('',#6593,#1605);
#1228=LINE('',#6599,#1606);
#1229=LINE('',#6605,#1607);
#1230=LINE('',#6611,#1608);
#1231=LINE('',#6617,#1609);
#1232=LINE('',#6634,#1610);
#1233=LINE('',#6639,#1611);
#1234=LINE('',#6643,#1612);
#1235=LINE('',#6648,#1613);
#1236=LINE('',#6651,#1614);
#1237=LINE('',#6657,#1615);
#1238=LINE('',#6660,#1616);
#1239=LINE('',#6665,#1617);
#1240=LINE('',#6667,#1618);
#1241=LINE('',#6669,#1619);
#1242=LINE('',#6670,#1620);
#1243=LINE('',#6674,#1621);
#1244=LINE('',#6675,#1622);
#1245=LINE('',#6676,#1623);
#1246=LINE('',#6680,#1624);
#1247=LINE('',#6681,#1625);
#1248=LINE('',#6682,#1626);
#1249=LINE('',#6687,#1627);
#1250=LINE('',#6699,#1628);
#1251=LINE('',#6703,#1629);
#1252=LINE('',#6712,#1630);
#1253=LINE('',#6713,#1631);
#1254=LINE('',#6716,#1632);
#1255=LINE('',#6718,#1633);
#1256=LINE('',#6719,#1634);
#1257=LINE('',#6722,#1635);
#1258=LINE('',#6723,#1636);
#1259=LINE('',#6726,#1637);
#1260=LINE('',#6727,#1638);
#1261=LINE('',#6729,#1639);
#1262=LINE('',#6764,#1640);
#1263=VECTOR('',#4440,371.);
#1264=VECTOR('',#4441,28.0000000000002);
#1265=VECTOR('',#4442,73.9999999999999);
#1266=VECTOR('',#4443,248.);
#1267=VECTOR('',#4444,1050.);
#1268=VECTOR('',#4445,248.);
#1269=VECTOR('',#4446,74.0000000000001);
#1270=VECTOR('',#4447,28.0000000000002);
#1271=VECTOR('',#4448,371.);
#1272=VECTOR('',#4449,29.0000000000002);
#1273=VECTOR('',#4450,160.);
#1274=VECTOR('',#4451,29.0000000000002);
#1275=VECTOR('',#4460,155.);
#1276=VECTOR('',#4461,320.);
#1277=VECTOR('',#4462,155.);
#1278=VECTOR('',#4463,320.);
#1279=VECTOR('',#4464,320.);
#1280=VECTOR('',#4465,155.);
#1281=VECTOR('',#4466,320.);
#1282=VECTOR('',#4467,155.);
#1283=VECTOR('',#4470,28.);
#1284=VECTOR('',#4471,502.);
#1285=VECTOR('',#4472,28.0000000000002);
#1286=VECTOR('',#4473,49.);
#1287=VECTOR('',#4474,600.);
#1288=VECTOR('',#4475,248.);
#1289=VECTOR('',#4476,48.9999999999998);
#1290=VECTOR('',#4479,371.);
#1291=VECTOR('',#4480,28.0000000000002);
#1292=VECTOR('',#4481,73.9999999999999);
#1293=VECTOR('',#4482,1050.);
#1294=VECTOR('',#4483,248.);
#1295=VECTOR('',#4484,73.9999999999999);
#1296=VECTOR('',#4485,28.0000000000002);
#1297=VECTOR('',#4486,371.);
#1298=VECTOR('',#4487,29.0000000000002);
#1299=VECTOR('',#4488,160.);
#1300=VECTOR('',#4489,29.0000000000002);
#1301=VECTOR('',#4492,502.);
#1302=VECTOR('',#4493,28.);
#1303=VECTOR('',#4494,49.0000000000001);
#1304=VECTOR('',#4495,600.);
#1305=VECTOR('',#4496,48.9999999999998);
#1306=VECTOR('',#4497,28.0000000000002);
#1307=VECTOR('',#4500,3.00000000000011);
#1308=VECTOR('',#4501,49.9999999999997);
#1309=VECTOR('',#4502,74.9999999999999);
#1310=VECTOR('',#4503,3.00000000000001);
#1311=VECTOR('',#4504,71.9999999999999);
#1312=VECTOR('',#4505,46.9999999999998);
#1313=VECTOR('',#4508,3.00000000000011);
#1314=VECTOR('',#4509,47.0000000000001);
#1315=VECTOR('',#4510,71.9999999999999);
#1316=VECTOR('',#4511,3.00000000000001);
#1317=VECTOR('',#4512,75.);
#1318=VECTOR('',#4513,50.0000000000001);
#1319=VECTOR('',#4516,370.);
#1320=VECTOR('',#4517,30.0000000000001);
#1321=VECTOR('',#4518,160.);
#1322=VECTOR('',#4519,30.0000000000001);
#1323=VECTOR('',#4520,370.);
#1324=VECTOR('',#4521,30.0000000000001);
#1325=VECTOR('',#4522,72.);
#1326=VECTOR('',#4523,247.);
#1327=VECTOR('',#4524,1044.);
#1328=VECTOR('',#4525,247.);
#1329=VECTOR('',#4526,71.9999999999999);
#1330=VECTOR('',#4527,30.0000000000001);
#1331=VECTOR('',#4528,155.);
#1332=VECTOR('',#4529,320.);
#1333=VECTOR('',#4530,155.);
#1334=VECTOR('',#4531,320.);
#1335=VECTOR('',#4540,320.);
#1336=VECTOR('',#4541,155.);
#1337=VECTOR('',#4542,320.);
#1338=VECTOR('',#4543,155.);
#1339=VECTOR('',#4546,3.00000000000001);
#1340=VECTOR('',#4547,160.);
#1341=VECTOR('',#4548,3.00000000000001);
#1342=VECTOR('',#4549,160.);
#1343=VECTOR('',#4552,3.00000000000001);
#1344=VECTOR('',#4553,160.);
#1345=VECTOR('',#4554,3.00000000000001);
#1346=VECTOR('',#4557,2.99999999999997);
#1347=VECTOR('',#4558,47.);
#1348=VECTOR('',#4559,3.00000000000001);
#1349=VECTOR('',#4560,75.);
#1350=VECTOR('',#4561,50.);
#1351=VECTOR('',#4564,3.00000000000001);
#1352=VECTOR('',#4565,49.9999999999998);
#1353=VECTOR('',#4566,75.);
#1354=VECTOR('',#4567,3.00000000000001);
#1355=VECTOR('',#4568,46.9999999999998);
#1356=VECTOR('',#4577,30.);
#1357=VECTOR('',#4578,247.);
#1358=VECTOR('',#4579,594.);
#1359=VECTOR('',#4580,30.0000000000001);
#1360=VECTOR('',#4581,500.);
#1361=VECTOR('',#4584,30.0000000000001);
#1362=VECTOR('',#4585,370.);
#1363=VECTOR('',#4586,30.0000000000001);
#1364=VECTOR('',#4587,247.);
#1365=VECTOR('',#4588,1044.);
#1366=VECTOR('',#4589,30.0000000000001);
#1367=VECTOR('',#4590,370.);
#1368=VECTOR('',#4591,30.0000000000001);
#1369=VECTOR('',#4594,30.);
#1370=VECTOR('',#4595,500.);
#1371=VECTOR('',#4596,30.0000000000001);
#1372=VECTOR('',#4597,594.);
#1373=VECTOR('',#4606,2.00000000000003);
#1374=VECTOR('',#4607,27.6040069435298);
#1375=VECTOR('',#4608,2.99999999999997);
#1376=VECTOR('',#4609,27.6040069435298);
#1377=VECTOR('',#4610,3.00000000000001);
#1378=VECTOR('',#4615,1.99999999999999);
#1379=VECTOR('',#4618,28.0000000000002);
#1380=VECTOR('',#4621,26.6040069435298);
#1381=VECTOR('',#4622,2.00000000000003);
#1382=VECTOR('',#4623,27.6040069435297);
#1383=VECTOR('',#4624,2.00000000000003);
#1384=VECTOR('',#4629,28.0000000000002);
#1385=VECTOR('',#4630,1.99999999999999);
#1386=VECTOR('',#4631,2.00000000000003);
#1387=VECTOR('',#4632,27.6040069435297);
#1388=VECTOR('',#4633,2.00000000000003);
#1389=VECTOR('',#4634,26.6040069435298);
#1390=VECTOR('',#4637,3.00000000000001);
#1391=VECTOR('',#4642,27.6040069435298);
#1392=VECTOR('',#4643,2.99999999999997);
#1393=VECTOR('',#4644,27.6040069435298);
#1394=VECTOR('',#4645,2.00000000000003);
#1395=VECTOR('',#4648,3.00000000000001);
#1396=VECTOR('',#4649,27.6040069435298);
#1397=VECTOR('',#4650,2.99999999999997);
#1398=VECTOR('',#4651,27.6040069435298);
#1399=VECTOR('',#4652,2.00000000000003);
#1400=VECTOR('',#4655,1.99999999999999);
#1401=VECTOR('',#4662,28.0000000000002);
#1402=VECTOR('',#4663,2.00000000000003);
#1403=VECTOR('',#4664,27.6040069435297);
#1404=VECTOR('',#4665,2.00000000000003);
#1405=VECTOR('',#4666,26.6040069435298);
#1406=VECTOR('',#4669,2.00000000000003);
#1407=VECTOR('',#4670,27.6040069435298);
#1408=VECTOR('',#4671,2.99999999999997);
#1409=VECTOR('',#4672,27.6040069435298);
#1410=VECTOR('',#4673,3.00000000000001);
#1411=VECTOR('',#4676,1.99999999999999);
#1412=VECTOR('',#4677,28.0000000000002);
#1413=VECTOR('',#4680,26.6040069435298);
#1414=VECTOR('',#4681,2.00000000000003);
#1415=VECTOR('',#4682,27.6040069435297);
#1416=VECTOR('',#4683,2.00000000000003);
#1417=VECTOR('',#4690,3.00000000000001);
#1418=VECTOR('',#4691,3.00000000000001);
#1419=VECTOR('',#4694,3.00000000000001);
#1420=VECTOR('',#4697,3.00000000000001);
#1421=VECTOR('',#4702,3.00000000000001);
#1422=VECTOR('',#4703,3.00000000000001);
#1423=VECTOR('',#4706,3.00000000000001);
#1424=VECTOR('',#4709,3.00000000000001);
#1425=VECTOR('',#4714,2.);
#1426=VECTOR('',#4717,2.);
#1427=VECTOR('',#4720,2.);
#1428=VECTOR('',#4723,2.);
#1429=VECTOR('',#4726,1.99999999999999);
#1430=VECTOR('',#4727,28.0000000000002);
#1431=VECTOR('',#4730,26.6040069435297);
#1432=VECTOR('',#4731,2.00000000000003);
#1433=VECTOR('',#4732,27.6040069435296);
#1434=VECTOR('',#4733,2.00000000000003);
#1435=VECTOR('',#4736,1.99999999999999);
#1436=VECTOR('',#4745,28.);
#1437=VECTOR('',#4746,2.00000000000003);
#1438=VECTOR('',#4747,27.6040069435296);
#1439=VECTOR('',#4748,2.00000000000003);
#1440=VECTOR('',#4749,26.6040069435297);
#1441=VECTOR('',#4752,2.00000000000003);
#1442=VECTOR('',#4753,28.);
#1443=VECTOR('',#4756,26.6040069435299);
#1444=VECTOR('',#4757,2.00000000000003);
#1445=VECTOR('',#4758,27.6040069435297);
#1446=VECTOR('',#4759,2.00000000000003);
#1447=VECTOR('',#4762,2.00000000000017);
#1448=VECTOR('',#4771,28.0000000000002);
#1449=VECTOR('',#4772,2.00000000000003);
#1450=VECTOR('',#4773,27.6040069435297);
#1451=VECTOR('',#4774,2.00000000000003);
#1452=VECTOR('',#4775,26.6040069435299);
#1453=VECTOR('',#4778,102.60400694353);
#1454=VECTOR('',#4779,2.00000000000003);
#1455=VECTOR('',#4780,102.60400694353);
#1456=VECTOR('',#4783,2.00000000000003);
#1457=VECTOR('',#4784,75.);
#1458=VECTOR('',#4787,50.);
#1459=VECTOR('',#4790,77.6040069435298);
#1460=VECTOR('',#4791,77.6040069435298);
#1461=VECTOR('',#4794,25.6040069435298);
#1462=VECTOR('',#4795,75.6040069435298);
#1463=VECTOR('',#4796,100.60400694353);
#1464=VECTOR('',#4797,25.6040069435297);
#1465=VECTOR('',#4798,75.);
#1466=VECTOR('',#4799,50.);
#1467=VECTOR('',#4804,2.00000000000003);
#1468=VECTOR('',#4805,75.);
#1469=VECTOR('',#4808,2.00000000000003);
#1470=VECTOR('',#4809,102.60400694353);
#1471=VECTOR('',#4810,102.60400694353);
#1472=VECTOR('',#4813,77.6040069435298);
#1473=VECTOR('',#4814,77.6040069435298);
#1474=VECTOR('',#4817,50.);
#1475=VECTOR('',#4820,25.6040069435299);
#1476=VECTOR('',#4821,49.9999999999999);
#1477=VECTOR('',#4822,74.9999999999999);
#1478=VECTOR('',#4823,25.6040069435297);
#1479=VECTOR('',#4824,100.60400694353);
#1480=VECTOR('',#4825,75.6040069435296);
#1481=VECTOR('',#4830,2.00000000000003);
#1482=VECTOR('',#4831,50.);
#1483=VECTOR('',#4834,2.00000000000003);
#1484=VECTOR('',#4835,77.6040069435298);
#1485=VECTOR('',#4836,77.6040069435298);
#1486=VECTOR('',#4839,102.60400694353);
#1487=VECTOR('',#4840,102.60400694353);
#1488=VECTOR('',#4843,75.0000000000001);
#1489=VECTOR('',#4846,25.6040069435297);
#1490=VECTOR('',#4847,74.9999999999999);
#1491=VECTOR('',#4848,50.);
#1492=VECTOR('',#4849,25.6040069435297);
#1493=VECTOR('',#4850,75.6040069435298);
#1494=VECTOR('',#4851,100.60400694353);
#1495=VECTOR('',#4856,2.00000000000003);
#1496=VECTOR('',#4857,75.0000000000001);
#1497=VECTOR('',#4860,2.00000000000003);
#1498=VECTOR('',#4861,102.60400694353);
#1499=VECTOR('',#4862,102.60400694353);
#1500=VECTOR('',#4865,77.6040069435298);
#1501=VECTOR('',#4866,77.6040069435298);
#1502=VECTOR('',#4869,50.);
#1503=VECTOR('',#4872,25.6040069435297);
#1504=VECTOR('',#4873,49.9999999999998);
#1505=VECTOR('',#4874,74.9999999999999);
#1506=VECTOR('',#4875,25.6040069435297);
#1507=VECTOR('',#4876,100.60400694353);
#1508=VECTOR('',#4877,75.6040069435296);
#1509=VECTOR('',#4882,160.);
#1510=VECTOR('',#4885,160.);
#1511=VECTOR('',#4886,160.);
#1512=VECTOR('',#4893,160.);
#1513=VECTOR('',#4894,160.);
#1514=VECTOR('',#4897,160.);
#1515=VECTOR('',#5064,35.);
#1516=VECTOR('',#5067,35.);
#1517=VECTOR('',#5072,195.);
#1518=VECTOR('',#5073,1.99999999999999);
#1519=VECTOR('',#5074,195.);
#1520=VECTOR('',#5075,1.99999999999999);
#1521=VECTOR('',#5078,360.);
#1522=VECTOR('',#5079,1.99999999999999);
#1523=VECTOR('',#5080,360.);
#1524=VECTOR('',#5083,195.);
#1525=VECTOR('',#5084,1.99999999999999);
#1526=VECTOR('',#5085,195.);
#1527=VECTOR('',#5088,360.);
#1528=VECTOR('',#5089,360.);
#1529=VECTOR('',#5094,216.);
#1530=VECTOR('',#5097,216.);
#1531=VECTOR('',#5100,216.);
#1532=VECTOR('',#5103,216.);
#1533=VECTOR('',#5106,216.);
#1534=VECTOR('',#5109,216.);
#1535=VECTOR('',#5112,216.);
#1536=VECTOR('',#5115,216.);
#1537=VECTOR('',#5118,216.);
#1538=VECTOR('',#5121,216.);
#1539=VECTOR('',#5132,216.);
#1540=VECTOR('',#5135,216.);
#1541=VECTOR('',#5138,216.);
#1542=VECTOR('',#5141,216.);
#1543=VECTOR('',#5144,216.);
#1544=VECTOR('',#5147,216.);
#1545=VECTOR('',#5150,216.);
#1546=VECTOR('',#5153,216.);
#1547=VECTOR('',#5156,216.);
#1548=VECTOR('',#5159,216.);
#1549=VECTOR('',#5172,2.);
#1550=VECTOR('',#5175,2.);
#1551=VECTOR('',#5178,2.);
#1552=VECTOR('',#5181,2.);
#1553=VECTOR('',#5184,1.99999999999999);
#1554=VECTOR('',#5185,1.99999999999999);
#1555=VECTOR('',#5188,1.99999999999999);
#1556=VECTOR('',#5191,1.99999999999999);
#1557=VECTOR('',#5196,1.99999999999999);
#1558=VECTOR('',#5197,1.99999999999999);
#1559=VECTOR('',#5200,1.99999999999999);
#1560=VECTOR('',#5203,1.99999999999999);
#1561=VECTOR('',#5208,1.99999999999999);
#1562=VECTOR('',#5209,1.99999999999999);
#1563=VECTOR('',#5212,1.99999999999999);
#1564=VECTOR('',#5215,1.99999999999999);
#1565=VECTOR('',#5220,1.99999999999999);
#1566=VECTOR('',#5221,1.99999999999999);
#1567=VECTOR('',#5224,1.99999999999999);
#1568=VECTOR('',#5227,1.99999999999999);
#1569=VECTOR('',#5232,1.99999999999999);
#1570=VECTOR('',#5233,1.99999999999999);
#1571=VECTOR('',#5236,1.99999999999999);
#1572=VECTOR('',#5239,1.99999999999999);
#1573=VECTOR('',#5254,25.);
#1574=VECTOR('',#5257,57.0000000000001);
#1575=VECTOR('',#5260,57.0000000000001);
#1576=VECTOR('',#5263,57.0000000000001);
#1577=VECTOR('',#5266,57.0000000000001);
#1578=VECTOR('',#5271,5.04504057306444);
#1579=VECTOR('',#5272,3.);
#1580=VECTOR('',#5273,5.04504057306444);
#1581=VECTOR('',#5274,5.04504057306444);
#1582=VECTOR('',#5275,3.);
#1583=VECTOR('',#5276,5.04504057306444);
#1584=VECTOR('',#5283,3.);
#1585=VECTOR('',#5284,5.04504057306444);
#1586=VECTOR('',#5285,5.04504057306444);
#1587=VECTOR('',#5288,57.0000000000001);
#1588=VECTOR('',#5291,57.0000000000001);
#1589=VECTOR('',#5296,5.04504057306444);
#1590=VECTOR('',#5297,3.);
#1591=VECTOR('',#5298,5.04504057306444);
#1592=VECTOR('',#5301,57.0000000000001);
#1593=VECTOR('',#5304,57.0000000000001);
#1594=VECTOR('',#5311,7.5);
#1595=VECTOR('',#5332,16.55);
#1596=VECTOR('',#5339,16.55);
#1597=VECTOR('',#5356,12.5);
#1598=VECTOR('',#5375,21.95);
#1599=VECTOR('',#5382,21.95);
#1600=VECTOR('',#5395,26.);
#1601=VECTOR('',#5412,130.);
#1602=VECTOR('',#5421,130.);
#1603=VECTOR('',#5428,5.);
#1604=VECTOR('',#5435,5.);
#1605=VECTOR('',#5442,5.);
#1606=VECTOR('',#5449,5.);
#1607=VECTOR('',#5456,5.);
#1608=VECTOR('',#5463,90.);
#1609=VECTOR('',#5470,90.);
#1610=VECTOR('',#5493,28.);
#1611=VECTOR('',#5498,25.);
#1612=VECTOR('',#5503,28.);
#1613=VECTOR('',#5512,5.);
#1614=VECTOR('',#5515,122.);
#1615=VECTOR('',#5522,130.);
#1616=VECTOR('',#5527,122.);
#1617=VECTOR('',#5532,493.558507170122);
#1618=VECTOR('',#5533,24.);
#1619=VECTOR('',#5534,493.558507170122);
#1620=VECTOR('',#5535,24.);
#1621=VECTOR('',#5538,493.558507170122);
#1622=VECTOR('',#5539,9.23760430703403);
#1623=VECTOR('',#5540,9.23760430703403);
#1624=VECTOR('',#5543,493.558507170122);
#1625=VECTOR('',#5544,14.762395692966);
#1626=VECTOR('',#5545,14.762395692966);
#1627=VECTOR('',#5550,24.);
#1628=VECTOR('',#5555,9.23760430703401);
#1629=VECTOR('',#5560,14.762395692966);
#1630=VECTOR('',#5561,9.237604307034);
#1631=VECTOR('',#5562,9.23760430703398);
#1632=VECTOR('',#5565,493.558507170122);
#1633=VECTOR('',#5566,24.);
#1634=VECTOR('',#5567,493.558507170122);
#1635=VECTOR('',#5570,493.558507170122);
#1636=VECTOR('',#5571,9.23760430703404);
#1637=VECTOR('',#5574,493.558507170122);
#1638=VECTOR('',#5575,14.762395692966);
#1639=VECTOR('',#5578,9.237604307034);
#1640=VECTOR('',#5591,9.23760430703399);
#1641=VERTEX_POINT('',#5610);
#1642=VERTEX_POINT('',#5611);
#1643=VERTEX_POINT('',#5613);
#1644=VERTEX_POINT('',#5615);
#1645=VERTEX_POINT('',#5617);
#1646=VERTEX_POINT('',#5619);
#1647=VERTEX_POINT('',#5621);
#1648=VERTEX_POINT('',#5623);
#1649=VERTEX_POINT('',#5625);
#1650=VERTEX_POINT('',#5627);
#1651=VERTEX_POINT('',#5629);
#1652=VERTEX_POINT('',#5631);
#1653=VERTEX_POINT('',#5634);
#1654=VERTEX_POINT('',#5636);
#1655=VERTEX_POINT('',#5638);
#1656=VERTEX_POINT('',#5640);
#1657=VERTEX_POINT('',#5642);
#1658=VERTEX_POINT('',#5643);
#1659=VERTEX_POINT('',#5645);
#1660=VERTEX_POINT('',#5647);
#1661=VERTEX_POINT('',#5650);
#1662=VERTEX_POINT('',#5651);
#1663=VERTEX_POINT('',#5653);
#1664=VERTEX_POINT('',#5655);
#1665=VERTEX_POINT('',#5659);
#1666=VERTEX_POINT('',#5660);
#1667=VERTEX_POINT('',#5662);
#1668=VERTEX_POINT('',#5664);
#1669=VERTEX_POINT('',#5667);
#1670=VERTEX_POINT('',#5669);
#1671=VERTEX_POINT('',#5673);
#1672=VERTEX_POINT('',#5674);
#1673=VERTEX_POINT('',#5676);
#1674=VERTEX_POINT('',#5679);
#1675=VERTEX_POINT('',#5681);
#1676=VERTEX_POINT('',#5683);
#1677=VERTEX_POINT('',#5685);
#1678=VERTEX_POINT('',#5687);
#1679=VERTEX_POINT('',#5689);
#1680=VERTEX_POINT('',#5691);
#1681=VERTEX_POINT('',#5695);
#1682=VERTEX_POINT('',#5696);
#1683=VERTEX_POINT('',#5698);
#1684=VERTEX_POINT('',#5702);
#1685=VERTEX_POINT('',#5706);
#1686=VERTEX_POINT('',#5707);
#1687=VERTEX_POINT('',#5709);
#1688=VERTEX_POINT('',#5711);
#1689=VERTEX_POINT('',#5713);
#1690=VERTEX_POINT('',#5715);
#1691=VERTEX_POINT('',#5719);
#1692=VERTEX_POINT('',#5720);
#1693=VERTEX_POINT('',#5722);
#1694=VERTEX_POINT('',#5724);
#1695=VERTEX_POINT('',#5726);
#1696=VERTEX_POINT('',#5728);
#1697=VERTEX_POINT('',#5732);
#1698=VERTEX_POINT('',#5733);
#1699=VERTEX_POINT('',#5735);
#1700=VERTEX_POINT('',#5737);
#1701=VERTEX_POINT('',#5739);
#1702=VERTEX_POINT('',#5741);
#1703=VERTEX_POINT('',#5743);
#1704=VERTEX_POINT('',#5745);
#1705=VERTEX_POINT('',#5747);
#1706=VERTEX_POINT('',#5749);
#1707=VERTEX_POINT('',#5751);
#1708=VERTEX_POINT('',#5753);
#1709=VERTEX_POINT('',#5756);
#1710=VERTEX_POINT('',#5757);
#1711=VERTEX_POINT('',#5759);
#1712=VERTEX_POINT('',#5761);
#1713=VERTEX_POINT('',#5764);
#1714=VERTEX_POINT('',#5766);
#1715=VERTEX_POINT('',#5768);
#1716=VERTEX_POINT('',#5770);
#1717=VERTEX_POINT('',#5772);
#1718=VERTEX_POINT('',#5773);
#1719=VERTEX_POINT('',#5775);
#1720=VERTEX_POINT('',#5777);
#1721=VERTEX_POINT('',#5781);
#1722=VERTEX_POINT('',#5782);
#1723=VERTEX_POINT('',#5784);
#1724=VERTEX_POINT('',#5786);
#1725=VERTEX_POINT('',#5790);
#1726=VERTEX_POINT('',#5792);
#1727=VERTEX_POINT('',#5796);
#1728=VERTEX_POINT('',#5797);
#1729=VERTEX_POINT('',#5800);
#1730=VERTEX_POINT('',#5802);
#1731=VERTEX_POINT('',#5806);
#1732=VERTEX_POINT('',#5807);
#1733=VERTEX_POINT('',#5809);
#1734=VERTEX_POINT('',#5811);
#1735=VERTEX_POINT('',#5816);
#1736=VERTEX_POINT('',#5818);
#1737=VERTEX_POINT('',#5821);
#1738=VERTEX_POINT('',#5823);
#1739=VERTEX_POINT('',#5826);
#1740=VERTEX_POINT('',#5830);
#1741=VERTEX_POINT('',#5832);
#1742=VERTEX_POINT('',#5835);
#1743=VERTEX_POINT('',#5838);
#1744=VERTEX_POINT('',#5840);
#1745=VERTEX_POINT('',#5844);
#1746=VERTEX_POINT('',#5846);
#1747=VERTEX_POINT('',#5851);
#1748=VERTEX_POINT('',#5853);
#1749=VERTEX_POINT('',#5856);
#1750=VERTEX_POINT('',#5858);
#1751=VERTEX_POINT('',#5860);
#1752=VERTEX_POINT('',#5865);
#1753=VERTEX_POINT('',#5869);
#1754=VERTEX_POINT('',#5871);
#1755=VERTEX_POINT('',#5873);
#1756=VERTEX_POINT('',#5875);
#1757=VERTEX_POINT('',#5877);
#1758=VERTEX_POINT('',#5881);
#1759=VERTEX_POINT('',#5882);
#1760=VERTEX_POINT('',#5884);
#1761=VERTEX_POINT('',#5887);
#1762=VERTEX_POINT('',#5889);
#1763=VERTEX_POINT('',#5891);
#1764=VERTEX_POINT('',#5898);
#1765=VERTEX_POINT('',#5900);
#1766=VERTEX_POINT('',#5902);
#1767=VERTEX_POINT('',#5907);
#1768=VERTEX_POINT('',#5909);
#1769=VERTEX_POINT('',#5911);
#1770=VERTEX_POINT('',#5915);
#1771=VERTEX_POINT('',#5919);
#1772=VERTEX_POINT('',#5920);
#1773=VERTEX_POINT('',#5923);
#1774=VERTEX_POINT('',#5925);
#1775=VERTEX_POINT('',#5927);
#1776=VERTEX_POINT('',#5931);
#1777=VERTEX_POINT('',#5933);
#1778=VERTEX_POINT('',#5935);
#1779=VERTEX_POINT('',#5940);
#1780=VERTEX_POINT('',#5942);
#1781=VERTEX_POINT('',#5944);
#1782=VERTEX_POINT('',#5946);
#1783=VERTEX_POINT('',#5948);
#1784=VERTEX_POINT('',#5950);
#1785=VERTEX_POINT('',#5980);
#1786=VERTEX_POINT('',#5982);
#1787=VERTEX_POINT('',#5984);
#1788=VERTEX_POINT('',#5986);
#1789=VERTEX_POINT('',#5988);
#1790=VERTEX_POINT('',#5990);
#1791=VERTEX_POINT('',#5994);
#1792=VERTEX_POINT('',#5999);
#1793=VERTEX_POINT('',#6000);
#1794=VERTEX_POINT('',#6003);
#1795=VERTEX_POINT('',#6005);
#1796=VERTEX_POINT('',#6007);
#1797=VERTEX_POINT('',#6011);
#1798=VERTEX_POINT('',#6013);
#1799=VERTEX_POINT('',#6015);
#1800=VERTEX_POINT('',#6017);
#1801=VERTEX_POINT('',#6019);
#1802=VERTEX_POINT('',#6021);
#1803=VERTEX_POINT('',#6025);
#1804=VERTEX_POINT('',#6030);
#1805=VERTEX_POINT('',#6031);
#1806=VERTEX_POINT('',#6034);
#1807=VERTEX_POINT('',#6036);
#1808=VERTEX_POINT('',#6038);
#1809=VERTEX_POINT('',#6042);
#1810=VERTEX_POINT('',#6044);
#1811=VERTEX_POINT('',#6048);
#1812=VERTEX_POINT('',#6057);
#1813=VERTEX_POINT('',#6058);
#1814=VERTEX_POINT('',#6060);
#1815=VERTEX_POINT('',#6062);
#1816=VERTEX_POINT('',#6064);
#1817=VERTEX_POINT('',#6066);
#1818=VERTEX_POINT('',#6071);
#1819=VERTEX_POINT('',#6075);
#1820=VERTEX_POINT('',#6076);
#1821=VERTEX_POINT('',#6086);
#1822=VERTEX_POINT('',#6087);
#1823=VERTEX_POINT('',#6089);
#1824=VERTEX_POINT('',#6091);
#1825=VERTEX_POINT('',#6093);
#1826=VERTEX_POINT('',#6095);
#1827=VERTEX_POINT('',#6100);
#1828=VERTEX_POINT('',#6104);
#1829=VERTEX_POINT('',#6105);
#1830=VERTEX_POINT('',#6115);
#1831=VERTEX_POINT('',#6116);
#1832=VERTEX_POINT('',#6118);
#1833=VERTEX_POINT('',#6120);
#1834=VERTEX_POINT('',#6122);
#1835=VERTEX_POINT('',#6124);
#1836=VERTEX_POINT('',#6129);
#1837=VERTEX_POINT('',#6133);
#1838=VERTEX_POINT('',#6134);
#1839=VERTEX_POINT('',#6144);
#1840=VERTEX_POINT('',#6145);
#1841=VERTEX_POINT('',#6147);
#1842=VERTEX_POINT('',#6149);
#1843=VERTEX_POINT('',#6151);
#1844=VERTEX_POINT('',#6153);
#1845=VERTEX_POINT('',#6257);
#1846=VERTEX_POINT('',#6258);
#1847=VERTEX_POINT('',#6260);
#1848=VERTEX_POINT('',#6262);
#1849=VERTEX_POINT('',#6266);
#1850=VERTEX_POINT('',#6268);
#1851=VERTEX_POINT('',#6272);
#1852=VERTEX_POINT('',#6274);
#1853=VERTEX_POINT('',#6281);
#1854=VERTEX_POINT('',#6282);
#1855=VERTEX_POINT('',#6284);
#1856=VERTEX_POINT('',#6286);
#1857=VERTEX_POINT('',#6289);
#1858=VERTEX_POINT('',#6290);
#1859=VERTEX_POINT('',#6292);
#1860=VERTEX_POINT('',#6294);
#1861=VERTEX_POINT('',#6297);
#1862=VERTEX_POINT('',#6298);
#1863=VERTEX_POINT('',#6300);
#1864=VERTEX_POINT('',#6302);
#1865=VERTEX_POINT('',#6305);
#1866=VERTEX_POINT('',#6306);
#1867=VERTEX_POINT('',#6308);
#1868=VERTEX_POINT('',#6310);
#1869=VERTEX_POINT('',#6313);
#1870=VERTEX_POINT('',#6314);
#1871=VERTEX_POINT('',#6316);
#1872=VERTEX_POINT('',#6318);
#1873=VERTEX_POINT('',#6321);
#1874=VERTEX_POINT('',#6323);
#1875=VERTEX_POINT('',#6325);
#1876=VERTEX_POINT('',#6327);
#1877=VERTEX_POINT('',#6330);
#1878=VERTEX_POINT('',#6331);
#1879=VERTEX_POINT('',#6333);
#1880=VERTEX_POINT('',#6335);
#1881=VERTEX_POINT('',#6338);
#1882=VERTEX_POINT('',#6339);
#1883=VERTEX_POINT('',#6341);
#1884=VERTEX_POINT('',#6343);
#1885=VERTEX_POINT('',#6346);
#1886=VERTEX_POINT('',#6347);
#1887=VERTEX_POINT('',#6349);
#1888=VERTEX_POINT('',#6351);
#1889=VERTEX_POINT('',#6354);
#1890=VERTEX_POINT('',#6355);
#1891=VERTEX_POINT('',#6357);
#1892=VERTEX_POINT('',#6359);
#1893=VERTEX_POINT('',#6362);
#1894=VERTEX_POINT('',#6363);
#1895=VERTEX_POINT('',#6365);
#1896=VERTEX_POINT('',#6367);
#1897=VERTEX_POINT('',#6370);
#1898=VERTEX_POINT('',#6372);
#1899=VERTEX_POINT('',#6374);
#1900=VERTEX_POINT('',#6376);
#1901=VERTEX_POINT('',#6431);
#1902=VERTEX_POINT('',#6433);
#1903=VERTEX_POINT('',#6435);
#1904=VERTEX_POINT('',#6437);
#1905=VERTEX_POINT('',#6439);
#1906=VERTEX_POINT('',#6441);
#1907=VERTEX_POINT('',#6443);
#1908=VERTEX_POINT('',#6445);
#1909=VERTEX_POINT('',#6447);
#1910=VERTEX_POINT('',#6449);
#1911=VERTEX_POINT('',#6453);
#1912=VERTEX_POINT('',#6455);
#1913=VERTEX_POINT('',#6458);
#1914=VERTEX_POINT('',#6460);
#1915=VERTEX_POINT('',#6463);
#1916=VERTEX_POINT('',#6467);
#1917=VERTEX_POINT('',#6468);
#1918=VERTEX_POINT('',#6478);
#1919=VERTEX_POINT('',#6480);
#1920=VERTEX_POINT('',#6489);
#1921=VERTEX_POINT('',#6495);
#1922=VERTEX_POINT('',#6496);
#1923=VERTEX_POINT('',#6498);
#1924=VERTEX_POINT('',#6500);
#1925=VERTEX_POINT('',#6505);
#1926=VERTEX_POINT('',#6509);
#1927=VERTEX_POINT('',#6510);
#1928=VERTEX_POINT('',#6513);
#1929=VERTEX_POINT('',#6517);
#1930=VERTEX_POINT('',#6520);
#1931=VERTEX_POINT('',#6524);
#1932=VERTEX_POINT('',#6528);
#1933=VERTEX_POINT('',#6533);
#1934=VERTEX_POINT('',#6535);
#1935=VERTEX_POINT('',#6539);
#1936=VERTEX_POINT('',#6543);
#1937=VERTEX_POINT('',#6547);
#1938=VERTEX_POINT('',#6550);
#1939=VERTEX_POINT('',#6554);
#1940=VERTEX_POINT('',#6558);
#1941=VERTEX_POINT('',#6564);
#1942=VERTEX_POINT('',#6566);
#1943=VERTEX_POINT('',#6570);
#1944=VERTEX_POINT('',#6571);
#1945=VERTEX_POINT('',#6574);
#1946=VERTEX_POINT('',#6578);
#1947=VERTEX_POINT('',#6580);
#1948=VERTEX_POINT('',#6584);
#1949=VERTEX_POINT('',#6586);
#1950=VERTEX_POINT('',#6590);
#1951=VERTEX_POINT('',#6592);
#1952=VERTEX_POINT('',#6596);
#1953=VERTEX_POINT('',#6598);
#1954=VERTEX_POINT('',#6602);
#1955=VERTEX_POINT('',#6604);
#1956=VERTEX_POINT('',#6608);
#1957=VERTEX_POINT('',#6610);
#1958=VERTEX_POINT('',#6614);
#1959=VERTEX_POINT('',#6616);
#1960=VERTEX_POINT('',#6622);
#1961=VERTEX_POINT('',#6624);
#1962=VERTEX_POINT('',#6627);
#1963=VERTEX_POINT('',#6629);
#1964=VERTEX_POINT('',#6632);
#1965=VERTEX_POINT('',#6636);
#1966=VERTEX_POINT('',#6638);
#1967=VERTEX_POINT('',#6642);
#1968=VERTEX_POINT('',#6650);
#1969=VERTEX_POINT('',#6652);
#1970=VERTEX_POINT('',#6656);
#1971=VERTEX_POINT('',#6663);
#1972=VERTEX_POINT('',#6664);
#1973=VERTEX_POINT('',#6666);
#1974=VERTEX_POINT('',#6668);
#1975=VERTEX_POINT('',#6672);
#1976=VERTEX_POINT('',#6673);
#1977=VERTEX_POINT('',#6678);
#1978=VERTEX_POINT('',#6679);
#1979=VERTEX_POINT('',#6684);
#1980=VERTEX_POINT('',#6686);
#1981=VERTEX_POINT('',#6697);
#1982=VERTEX_POINT('',#6701);
#1983=VERTEX_POINT('',#6715);
#1984=VERTEX_POINT('',#6717);
#1985=VERTEX_POINT('',#6721);
#1986=VERTEX_POINT('',#6725);
#1987=EDGE_CURVE('',#1641,#1642,#885,.T.);
#1988=EDGE_CURVE('',#1641,#1643,#886,.F.);
#1989=EDGE_CURVE('',#1643,#1644,#887,.T.);
#1990=EDGE_CURVE('',#1644,#1645,#888,.T.);
#1991=EDGE_CURVE('',#1646,#1645,#889,.T.);
#1992=EDGE_CURVE('',#1647,#1646,#890,.T.);
#1993=EDGE_CURVE('',#1647,#1648,#891,.T.);
#1994=EDGE_CURVE('',#1648,#1649,#892,.F.);
#1995=EDGE_CURVE('',#1650,#1649,#893,.T.);
#1996=EDGE_CURVE('',#1651,#1650,#894,.T.);
#1997=EDGE_CURVE('',#1651,#1652,#895,.T.);
#1998=EDGE_CURVE('',#1642,#1652,#896,.T.);
#1999=EDGE_CURVE('',#1653,#1653,#242,.T.);
#2000=EDGE_CURVE('',#1654,#1654,#243,.T.);
#2001=EDGE_CURVE('',#1655,#1655,#244,.T.);
#2002=EDGE_CURVE('',#1656,#1656,#245,.T.);
#2003=EDGE_CURVE('',#1657,#1658,#897,.T.);
#2004=EDGE_CURVE('',#1657,#1659,#898,.T.);
#2005=EDGE_CURVE('',#1659,#1660,#899,.T.);
#2006=EDGE_CURVE('',#1658,#1660,#900,.T.);
#2007=EDGE_CURVE('',#1661,#1662,#901,.T.);
#2008=EDGE_CURVE('',#1661,#1663,#902,.T.);
#2009=EDGE_CURVE('',#1663,#1664,#903,.T.);
#2010=EDGE_CURVE('',#1662,#1664,#904,.T.);
#2011=EDGE_CURVE('',#1665,#1666,#905,.T.);
#2012=EDGE_CURVE('',#1666,#1667,#906,.T.);
#2013=EDGE_CURVE('',#1667,#1668,#907,.T.);
#2014=EDGE_CURVE('',#1668,#1647,#908,.T.);
#2015=EDGE_CURVE('',#1646,#1669,#909,.T.);
#2016=EDGE_CURVE('',#1670,#1669,#910,.T.);
#2017=EDGE_CURVE('',#1670,#1665,#911,.T.);
#2018=EDGE_CURVE('',#1671,#1672,#912,.T.);
#2019=EDGE_CURVE('',#1672,#1673,#913,.T.);
#2020=EDGE_CURVE('',#1673,#1670,#914,.T.);
#2021=EDGE_CURVE('',#1669,#1674,#915,.T.);
#2022=EDGE_CURVE('',#1675,#1674,#916,.T.);
#2023=EDGE_CURVE('',#1675,#1676,#917,.T.);
#2024=EDGE_CURVE('',#1676,#1677,#918,.T.);
#2025=EDGE_CURVE('',#1677,#1678,#919,.T.);
#2026=EDGE_CURVE('',#1678,#1679,#920,.T.);
#2027=EDGE_CURVE('',#1679,#1680,#921,.T.);
#2028=EDGE_CURVE('',#1680,#1671,#922,.T.);
#2029=EDGE_CURVE('',#1681,#1682,#923,.T.);
#2030=EDGE_CURVE('',#1682,#1683,#924,.T.);
#2031=EDGE_CURVE('',#1683,#1675,#925,.T.);
#2032=EDGE_CURVE('',#1645,#1674,#926,.T.);
#2033=EDGE_CURVE('',#1644,#1684,#927,.T.);
#2034=EDGE_CURVE('',#1684,#1681,#928,.T.);
#2035=EDGE_CURVE('',#1685,#1686,#929,.T.);
#2036=EDGE_CURVE('',#1685,#1687,#930,.T.);
#2037=EDGE_CURVE('',#1687,#1688,#931,.T.);
#2038=EDGE_CURVE('',#1689,#1688,#932,.T.);
#2039=EDGE_CURVE('',#1690,#1689,#933,.T.);
#2040=EDGE_CURVE('',#1686,#1690,#934,.T.);
#2041=EDGE_CURVE('',#1691,#1692,#935,.T.);
#2042=EDGE_CURVE('',#1691,#1693,#936,.T.);
#2043=EDGE_CURVE('',#1694,#1693,#937,.T.);
#2044=EDGE_CURVE('',#1695,#1694,#938,.T.);
#2045=EDGE_CURVE('',#1695,#1696,#939,.T.);
#2046=EDGE_CURVE('',#1692,#1696,#940,.T.);
#2047=EDGE_CURVE('',#1697,#1698,#941,.T.);
#2048=EDGE_CURVE('',#1698,#1699,#942,.T.);
#2049=EDGE_CURVE('',#1700,#1699,#943,.T.);
#2050=EDGE_CURVE('',#1700,#1701,#944,.T.);
#2051=EDGE_CURVE('',#1701,#1702,#945,.T.);
#2052=EDGE_CURVE('',#1702,#1703,#946,.T.);
#2053=EDGE_CURVE('',#1704,#1703,#947,.T.);
#2054=EDGE_CURVE('',#1704,#1705,#948,.T.);
#2055=EDGE_CURVE('',#1705,#1706,#949,.T.);
#2056=EDGE_CURVE('',#1707,#1706,#950,.T.);
#2057=EDGE_CURVE('',#1708,#1707,#951,.T.);
#2058=EDGE_CURVE('',#1708,#1697,#952,.T.);
#2059=EDGE_CURVE('',#1709,#1710,#953,.T.);
#2060=EDGE_CURVE('',#1709,#1711,#954,.T.);
#2061=EDGE_CURVE('',#1711,#1712,#955,.T.);
#2062=EDGE_CURVE('',#1710,#1712,#956,.T.);
#2063=EDGE_CURVE('',#1713,#1713,#246,.T.);
#2064=EDGE_CURVE('',#1714,#1714,#247,.T.);
#2065=EDGE_CURVE('',#1715,#1715,#248,.T.);
#2066=EDGE_CURVE('',#1716,#1716,#249,.T.);
#2067=EDGE_CURVE('',#1717,#1718,#957,.T.);
#2068=EDGE_CURVE('',#1717,#1719,#958,.T.);
#2069=EDGE_CURVE('',#1719,#1720,#959,.T.);
#2070=EDGE_CURVE('',#1718,#1720,#960,.T.);
#2071=EDGE_CURVE('',#1721,#1722,#961,.T.);
#2072=EDGE_CURVE('',#1723,#1721,#962,.T.);
#2073=EDGE_CURVE('',#1724,#1723,#963,.T.);
#2074=EDGE_CURVE('',#1724,#1722,#964,.T.);
#2075=EDGE_CURVE('',#1725,#1699,#965,.T.);
#2076=EDGE_CURVE('',#1726,#1725,#966,.T.);
#2077=EDGE_CURVE('',#1700,#1726,#967,.T.);
#2078=EDGE_CURVE('',#1727,#1728,#968,.T.);
#2079=EDGE_CURVE('',#1704,#1727,#969,.T.);
#2080=EDGE_CURVE('',#1729,#1703,#970,.T.);
#2081=EDGE_CURVE('',#1730,#1729,#971,.T.);
#2082=EDGE_CURVE('',#1730,#1728,#972,.T.);
#2083=EDGE_CURVE('',#1731,#1732,#973,.T.);
#2084=EDGE_CURVE('',#1733,#1731,#974,.T.);
#2085=EDGE_CURVE('',#1734,#1733,#975,.T.);
#2086=EDGE_CURVE('',#1708,#1734,#976,.T.);
#2087=EDGE_CURVE('',#1707,#1732,#977,.T.);
#2088=EDGE_CURVE('',#1735,#1735,#250,.T.);
#2089=EDGE_CURVE('',#1736,#1736,#251,.T.);
#2090=EDGE_CURVE('',#1686,#1737,#978,.T.);
#2091=EDGE_CURVE('',#1690,#1738,#979,.T.);
#2092=EDGE_CURVE('',#1705,#1738,#980,.T.);
#2093=EDGE_CURVE('',#1739,#1727,#981,.T.);
#2094=EDGE_CURVE('',#1737,#1739,#982,.T.);
#2095=EDGE_CURVE('',#1740,#1721,#983,.T.);
#2096=EDGE_CURVE('',#1741,#1740,#984,.T.);
#2097=EDGE_CURVE('',#1694,#1741,#985,.T.);
#2098=EDGE_CURVE('',#1693,#1742,#986,.T.);
#2099=EDGE_CURVE('',#1738,#1742,#987,.T.);
#2100=EDGE_CURVE('',#1743,#1689,#988,.T.);
#2101=EDGE_CURVE('',#1744,#1743,#989,.T.);
#2102=EDGE_CURVE('',#1723,#1744,#990,.T.);
#2103=EDGE_CURVE('',#1691,#1745,#991,.T.);
#2104=EDGE_CURVE('',#1745,#1746,#992,.T.);
#2105=EDGE_CURVE('',#1746,#1732,#993,.T.);
#2106=EDGE_CURVE('',#1706,#1742,#994,.T.);
#2107=EDGE_CURVE('',#1747,#1747,#252,.T.);
#2108=EDGE_CURVE('',#1748,#1748,#253,.T.);
#2109=EDGE_CURVE('',#1726,#1749,#995,.T.);
#2110=EDGE_CURVE('',#1750,#1749,#996,.T.);
#2111=EDGE_CURVE('',#1751,#1750,#997,.T.);
#2112=EDGE_CURVE('',#1751,#1651,#998,.T.);
#2113=EDGE_CURVE('',#1701,#1650,#999,.T.);
#2114=EDGE_CURVE('',#1649,#1752,#254,.T.);
#2115=EDGE_CURVE('',#1702,#1752,#1000,.T.);
#2116=EDGE_CURVE('',#1752,#1753,#1001,.T.);
#2117=EDGE_CURVE('',#1754,#1753,#255,.F.);
#2118=EDGE_CURVE('',#1754,#1755,#1002,.T.);
#2119=EDGE_CURVE('',#1755,#1756,#1003,.T.);
#2120=EDGE_CURVE('',#1757,#1756,#1004,.T.);
#2121=EDGE_CURVE('',#1729,#1757,#1005,.T.);
#2122=EDGE_CURVE('',#1758,#1759,#256,.F.);
#2123=EDGE_CURVE('',#1758,#1760,#1006,.T.);
#2124=EDGE_CURVE('',#1697,#1760,#1007,.T.);
#2125=EDGE_CURVE('',#1734,#1761,#1008,.T.);
#2126=EDGE_CURVE('',#1762,#1761,#1009,.T.);
#2127=EDGE_CURVE('',#1763,#1762,#1010,.T.);
#2128=EDGE_CURVE('',#1763,#1759,#1011,.T.);
#2129=EDGE_CURVE('',#1698,#1642,#1012,.T.);
#2130=EDGE_CURVE('',#1760,#1641,#257,.T.);
#2131=EDGE_CURVE('',#1652,#1764,#1013,.T.);
#2132=EDGE_CURVE('',#1764,#1765,#1014,.T.);
#2133=EDGE_CURVE('',#1766,#1765,#1015,.T.);
#2134=EDGE_CURVE('',#1725,#1766,#1016,.T.);
#2135=EDGE_CURVE('',#1671,#1744,#1017,.T.);
#2136=EDGE_CURVE('',#1680,#1767,#1018,.T.);
#2137=EDGE_CURVE('',#1767,#1768,#1019,.T.);
#2138=EDGE_CURVE('',#1769,#1768,#1020,.T.);
#2139=EDGE_CURVE('',#1724,#1769,#1021,.T.);
#2140=EDGE_CURVE('',#1770,#1743,#1022,.T.);
#2141=EDGE_CURVE('',#1770,#1672,#258,.T.);
#2142=EDGE_CURVE('',#1771,#1772,#259,.F.);
#2143=EDGE_CURVE('',#1771,#1770,#1023,.F.);
#2144=EDGE_CURVE('',#1688,#1773,#1024,.T.);
#2145=EDGE_CURVE('',#1774,#1773,#1025,.T.);
#2146=EDGE_CURVE('',#1775,#1774,#1026,.T.);
#2147=EDGE_CURVE('',#1775,#1772,#1027,.T.);
#2148=EDGE_CURVE('',#1722,#1776,#1028,.T.);
#2149=EDGE_CURVE('',#1777,#1776,#1029,.T.);
#2150=EDGE_CURVE('',#1778,#1777,#1030,.T.);
#2151=EDGE_CURVE('',#1778,#1679,#1031,.T.);
#2152=EDGE_CURVE('',#1678,#1740,#1032,.T.);
#2153=EDGE_CURVE('',#1779,#1741,#1033,.T.);
#2154=EDGE_CURVE('',#1779,#1780,#1034,.F.);
#2155=EDGE_CURVE('',#1781,#1780,#260,.F.);
#2156=EDGE_CURVE('',#1781,#1782,#1035,.T.);
#2157=EDGE_CURVE('',#1782,#1783,#1036,.T.);
#2158=EDGE_CURVE('',#1784,#1783,#1037,.T.);
#2159=EDGE_CURVE('',#1695,#1784,#1038,.T.);
#2160=EDGE_CURVE('',#1677,#1779,#261,.T.);
#2161=EDGE_CURVE('',#1718,#1659,#1039,.T.);
#2162=EDGE_CURVE('',#1717,#1657,#1040,.T.);
#2163=EDGE_CURVE('',#1720,#1660,#1041,.T.);
#2164=EDGE_CURVE('',#1719,#1658,#1042,.T.);
#2165=EDGE_CURVE('',#1710,#1663,#1043,.T.);
#2166=EDGE_CURVE('',#1709,#1661,#1044,.T.);
#2167=EDGE_CURVE('',#1712,#1664,#1045,.T.);
#2168=EDGE_CURVE('',#1711,#1662,#1046,.T.);
#2169=EDGE_CURVE('',#1716,#1656,#1047,.T.);
#2170=EDGE_CURVE('',#1715,#1655,#1048,.T.);
#2171=EDGE_CURVE('',#1714,#1654,#1049,.T.);
#2172=EDGE_CURVE('',#1713,#1653,#1050,.T.);
#2173=EDGE_CURVE('',#1785,#1746,#1051,.T.);
#2174=EDGE_CURVE('',#1785,#1786,#1052,.F.);
#2175=EDGE_CURVE('',#1787,#1786,#262,.F.);
#2176=EDGE_CURVE('',#1787,#1788,#1053,.T.);
#2177=EDGE_CURVE('',#1788,#1789,#1054,.T.);
#2178=EDGE_CURVE('',#1790,#1789,#1055,.T.);
#2179=EDGE_CURVE('',#1731,#1790,#1056,.T.);
#2180=EDGE_CURVE('',#1791,#1745,#1057,.T.);
#2181=EDGE_CURVE('',#1791,#1682,#263,.T.);
#2182=EDGE_CURVE('',#1681,#1785,#264,.T.);
#2183=EDGE_CURVE('',#1792,#1793,#265,.F.);
#2184=EDGE_CURVE('',#1792,#1791,#1058,.F.);
#2185=EDGE_CURVE('',#1692,#1794,#1059,.T.);
#2186=EDGE_CURVE('',#1795,#1794,#1060,.T.);
#2187=EDGE_CURVE('',#1796,#1795,#1061,.T.);
#2188=EDGE_CURVE('',#1796,#1793,#1062,.T.);
#2189=EDGE_CURVE('',#1737,#1797,#1063,.T.);
#2190=EDGE_CURVE('',#1797,#1798,#1064,.F.);
#2191=EDGE_CURVE('',#1799,#1798,#266,.F.);
#2192=EDGE_CURVE('',#1799,#1800,#1065,.T.);
#2193=EDGE_CURVE('',#1800,#1801,#1066,.T.);
#2194=EDGE_CURVE('',#1802,#1801,#1067,.T.);
#2195=EDGE_CURVE('',#1685,#1802,#1068,.T.);
#2196=EDGE_CURVE('',#1739,#1803,#1069,.T.);
#2197=EDGE_CURVE('',#1803,#1667,#267,.T.);
#2198=EDGE_CURVE('',#1666,#1797,#268,.T.);
#2199=EDGE_CURVE('',#1804,#1805,#269,.F.);
#2200=EDGE_CURVE('',#1804,#1803,#1070,.F.);
#2201=EDGE_CURVE('',#1728,#1806,#1071,.T.);
#2202=EDGE_CURVE('',#1807,#1806,#1072,.T.);
#2203=EDGE_CURVE('',#1808,#1807,#1073,.T.);
#2204=EDGE_CURVE('',#1808,#1805,#1074,.T.);
#2205=EDGE_CURVE('',#1755,#1809,#1075,.T.);
#2206=EDGE_CURVE('',#1809,#1810,#1076,.T.);
#2207=EDGE_CURVE('',#1756,#1810,#1077,.T.);
#2208=EDGE_CURVE('',#1730,#1811,#1078,.T.);
#2209=EDGE_CURVE('',#1811,#1757,#1079,.T.);
#2210=EDGE_CURVE('',#1806,#1811,#1080,.T.);
#2211=EDGE_CURVE('',#1809,#1808,#1081,.T.);
#2212=EDGE_CURVE('',#1810,#1807,#1082,.T.);
#2213=EDGE_CURVE('',#1812,#1813,#1083,.F.);
#2214=EDGE_CURVE('',#1813,#1814,#1084,.F.);
#2215=EDGE_CURVE('',#1814,#1815,#1085,.F.);
#2216=EDGE_CURVE('',#1815,#1816,#1086,.F.);
#2217=EDGE_CURVE('',#1816,#1817,#1087,.F.);
#2218=EDGE_CURVE('',#1817,#1812,#1088,.F.);
#2219=EDGE_CURVE('',#1687,#1818,#1089,.T.);
#2220=EDGE_CURVE('',#1773,#1818,#1090,.T.);
#2221=EDGE_CURVE('',#1819,#1820,#1091,.T.);
#2222=EDGE_CURVE('',#1819,#1775,#1092,.T.);
#2223=EDGE_CURVE('',#1820,#1774,#1093,.T.);
#2224=EDGE_CURVE('',#1800,#1819,#1094,.T.);
#2225=EDGE_CURVE('',#1801,#1820,#1095,.T.);
#2226=EDGE_CURVE('',#1818,#1802,#1096,.T.);
#2227=EDGE_CURVE('',#1821,#1822,#1097,.F.);
#2228=EDGE_CURVE('',#1822,#1823,#1098,.F.);
#2229=EDGE_CURVE('',#1823,#1824,#1099,.F.);
#2230=EDGE_CURVE('',#1824,#1825,#1100,.F.);
#2231=EDGE_CURVE('',#1825,#1826,#1101,.F.);
#2232=EDGE_CURVE('',#1826,#1821,#1102,.F.);
#2233=EDGE_CURVE('',#1696,#1827,#1103,.T.);
#2234=EDGE_CURVE('',#1794,#1827,#1104,.T.);
#2235=EDGE_CURVE('',#1828,#1829,#1105,.T.);
#2236=EDGE_CURVE('',#1828,#1796,#1106,.T.);
#2237=EDGE_CURVE('',#1829,#1795,#1107,.T.);
#2238=EDGE_CURVE('',#1782,#1828,#1108,.T.);
#2239=EDGE_CURVE('',#1783,#1829,#1109,.T.);
#2240=EDGE_CURVE('',#1827,#1784,#1110,.T.);
#2241=EDGE_CURVE('',#1830,#1831,#1111,.F.);
#2242=EDGE_CURVE('',#1831,#1832,#1112,.F.);
#2243=EDGE_CURVE('',#1832,#1833,#1113,.F.);
#2244=EDGE_CURVE('',#1833,#1834,#1114,.F.);
#2245=EDGE_CURVE('',#1834,#1835,#1115,.F.);
#2246=EDGE_CURVE('',#1835,#1830,#1116,.F.);
#2247=EDGE_CURVE('',#1733,#1836,#1117,.T.);
#2248=EDGE_CURVE('',#1761,#1836,#1118,.T.);
#2249=EDGE_CURVE('',#1837,#1838,#1119,.T.);
#2250=EDGE_CURVE('',#1837,#1763,#1120,.T.);
#2251=EDGE_CURVE('',#1838,#1762,#1121,.T.);
#2252=EDGE_CURVE('',#1788,#1837,#1122,.T.);
#2253=EDGE_CURVE('',#1789,#1838,#1123,.T.);
#2254=EDGE_CURVE('',#1836,#1790,#1124,.T.);
#2255=EDGE_CURVE('',#1839,#1840,#1125,.F.);
#2256=EDGE_CURVE('',#1840,#1841,#1126,.F.);
#2257=EDGE_CURVE('',#1841,#1842,#1127,.F.);
#2258=EDGE_CURVE('',#1842,#1843,#1128,.F.);
#2259=EDGE_CURVE('',#1843,#1844,#1129,.F.);
#2260=EDGE_CURVE('',#1844,#1839,#1130,.F.);
#2261=EDGE_CURVE('',#1776,#1769,#1131,.T.);
#2262=EDGE_CURVE('',#1768,#1777,#1132,.T.);
#2263=EDGE_CURVE('',#1767,#1778,#1133,.T.);
#2264=EDGE_CURVE('',#1765,#1750,#1134,.T.);
#2265=EDGE_CURVE('',#1764,#1751,#1135,.T.);
#2266=EDGE_CURVE('',#1749,#1766,#1136,.T.);
#2267=EDGE_CURVE('',#1772,#1824,#270,.T.);
#2268=EDGE_CURVE('',#1825,#1775,#92,.T.);
#2269=EDGE_CURVE('',#1673,#1771,#271,.T.);
#2270=EDGE_CURVE('',#1826,#1819,#93,.F.);
#2271=EDGE_CURVE('',#1673,#1824,#272,.F.);
#2272=EDGE_CURVE('',#1821,#1800,#94,.F.);
#2273=EDGE_CURVE('',#1670,#1823,#95,.F.);
#2274=EDGE_CURVE('',#1822,#1799,#273,.T.);
#2275=EDGE_CURVE('',#1665,#1822,#274,.T.);
#2276=EDGE_CURVE('',#1665,#1798,#275,.F.);
#2277=EDGE_CURVE('',#1793,#1833,#276,.T.);
#2278=EDGE_CURVE('',#1834,#1796,#96,.F.);
#2279=EDGE_CURVE('',#1683,#1792,#277,.T.);
#2280=EDGE_CURVE('',#1835,#1828,#97,.T.);
#2281=EDGE_CURVE('',#1683,#1833,#278,.F.);
#2282=EDGE_CURVE('',#1830,#1782,#98,.T.);
#2283=EDGE_CURVE('',#1675,#1832,#99,.F.);
#2284=EDGE_CURVE('',#1831,#1781,#279,.T.);
#2285=EDGE_CURVE('',#1676,#1831,#280,.T.);
#2286=EDGE_CURVE('',#1676,#1780,#281,.F.);
#2287=EDGE_CURVE('',#1759,#1842,#282,.T.);
#2288=EDGE_CURVE('',#1843,#1763,#100,.T.);
#2289=EDGE_CURVE('',#1643,#1758,#283,.T.);
#2290=EDGE_CURVE('',#1844,#1837,#101,.F.);
#2291=EDGE_CURVE('',#1643,#1842,#284,.F.);
#2292=EDGE_CURVE('',#1839,#1788,#102,.F.);
#2293=EDGE_CURVE('',#1644,#1841,#103,.T.);
#2294=EDGE_CURVE('',#1840,#1787,#285,.T.);
#2295=EDGE_CURVE('',#1684,#1840,#286,.T.);
#2296=EDGE_CURVE('',#1684,#1786,#287,.F.);
#2297=EDGE_CURVE('',#1753,#1648,#288,.T.);
#2298=EDGE_CURVE('',#1755,#1815,#104,.F.);
#2299=EDGE_CURVE('',#1816,#1754,#289,.T.);
#2300=EDGE_CURVE('',#1816,#1648,#290,.F.);
#2301=EDGE_CURVE('',#1809,#1814,#105,.F.);
#2302=EDGE_CURVE('',#1817,#1647,#106,.T.);
#2303=EDGE_CURVE('',#1808,#1813,#107,.T.);
#2304=EDGE_CURVE('',#1812,#1668,#291,.T.);
#2305=EDGE_CURVE('',#1805,#1812,#292,.T.);
#2306=EDGE_CURVE('',#1804,#1668,#293,.F.);
#2307=EDGE_CURVE('',#1736,#1748,#1137,.T.);
#2308=EDGE_CURVE('',#1735,#1747,#1138,.T.);
#2309=EDGE_CURVE('',#1845,#1846,#1139,.T.);
#2310=EDGE_CURVE('',#1847,#1846,#1140,.T.);
#2311=EDGE_CURVE('',#1848,#1847,#1141,.T.);
#2312=EDGE_CURVE('',#1848,#1845,#1142,.T.);
#2313=EDGE_CURVE('',#1846,#1849,#1143,.T.);
#2314=EDGE_CURVE('',#1850,#1849,#1144,.T.);
#2315=EDGE_CURVE('',#1847,#1850,#1145,.T.);
#2316=EDGE_CURVE('',#1851,#1849,#1146,.T.);
#2317=EDGE_CURVE('',#1852,#1851,#1147,.T.);
#2318=EDGE_CURVE('',#1852,#1850,#1148,.T.);
#2319=EDGE_CURVE('',#1845,#1851,#1149,.T.);
#2320=EDGE_CURVE('',#1848,#1852,#1150,.T.);
#2321=EDGE_CURVE('',#1853,#1854,#294,.T.);
#2322=EDGE_CURVE('',#1855,#1853,#1151,.T.);
#2323=EDGE_CURVE('',#1856,#1855,#295,.T.);
#2324=EDGE_CURVE('',#1854,#1856,#1152,.T.);
#2325=EDGE_CURVE('',#1857,#1858,#296,.T.);
#2326=EDGE_CURVE('',#1859,#1857,#1153,.T.);
#2327=EDGE_CURVE('',#1860,#1859,#297,.T.);
#2328=EDGE_CURVE('',#1858,#1860,#1154,.T.);
#2329=EDGE_CURVE('',#1861,#1862,#298,.T.);
#2330=EDGE_CURVE('',#1863,#1861,#1155,.T.);
#2331=EDGE_CURVE('',#1864,#1863,#299,.T.);
#2332=EDGE_CURVE('',#1862,#1864,#1156,.T.);
#2333=EDGE_CURVE('',#1865,#1866,#300,.T.);
#2334=EDGE_CURVE('',#1867,#1865,#1157,.T.);
#2335=EDGE_CURVE('',#1868,#1867,#301,.T.);
#2336=EDGE_CURVE('',#1866,#1868,#1158,.T.);
#2337=EDGE_CURVE('',#1869,#1870,#302,.T.);
#2338=EDGE_CURVE('',#1871,#1869,#1159,.T.);
#2339=EDGE_CURVE('',#1872,#1871,#303,.T.);
#2340=EDGE_CURVE('',#1870,#1872,#1160,.T.);
#2341=EDGE_CURVE('',#1873,#1873,#304,.T.);
#2342=EDGE_CURVE('',#1874,#1874,#305,.T.);
#2343=EDGE_CURVE('',#1875,#1875,#306,.T.);
#2344=EDGE_CURVE('',#1876,#1876,#307,.T.);
#2345=EDGE_CURVE('',#1877,#1878,#1161,.T.);
#2346=EDGE_CURVE('',#1878,#1879,#308,.T.);
#2347=EDGE_CURVE('',#1879,#1880,#1162,.T.);
#2348=EDGE_CURVE('',#1880,#1877,#309,.T.);
#2349=EDGE_CURVE('',#1881,#1882,#1163,.T.);
#2350=EDGE_CURVE('',#1882,#1883,#310,.T.);
#2351=EDGE_CURVE('',#1883,#1884,#1164,.T.);
#2352=EDGE_CURVE('',#1884,#1881,#311,.T.);
#2353=EDGE_CURVE('',#1885,#1886,#1165,.T.);
#2354=EDGE_CURVE('',#1886,#1887,#312,.T.);
#2355=EDGE_CURVE('',#1887,#1888,#1166,.T.);
#2356=EDGE_CURVE('',#1888,#1885,#313,.T.);
#2357=EDGE_CURVE('',#1889,#1890,#1167,.T.);
#2358=EDGE_CURVE('',#1890,#1891,#314,.T.);
#2359=EDGE_CURVE('',#1891,#1892,#1168,.T.);
#2360=EDGE_CURVE('',#1892,#1889,#315,.T.);
#2361=EDGE_CURVE('',#1893,#1894,#1169,.T.);
#2362=EDGE_CURVE('',#1894,#1895,#316,.T.);
#2363=EDGE_CURVE('',#1895,#1896,#1170,.T.);
#2364=EDGE_CURVE('',#1896,#1893,#317,.T.);
#2365=EDGE_CURVE('',#1897,#1897,#318,.T.);
#2366=EDGE_CURVE('',#1898,#1898,#319,.T.);
#2367=EDGE_CURVE('',#1899,#1899,#320,.T.);
#2368=EDGE_CURVE('',#1900,#1900,#321,.T.);
#2369=EDGE_CURVE('',#1900,#1876,#1171,.T.);
#2370=EDGE_CURVE('',#1899,#1875,#1172,.T.);
#2371=EDGE_CURVE('',#1898,#1874,#1173,.T.);
#2372=EDGE_CURVE('',#1897,#1873,#1174,.T.);
#2373=EDGE_CURVE('',#1894,#1869,#1175,.T.);
#2374=EDGE_CURVE('',#1895,#1870,#1176,.T.);
#2375=EDGE_CURVE('',#1893,#1871,#1177,.T.);
#2376=EDGE_CURVE('',#1896,#1872,#1178,.T.);
#2377=EDGE_CURVE('',#1890,#1865,#1179,.T.);
#2378=EDGE_CURVE('',#1891,#1866,#1180,.T.);
#2379=EDGE_CURVE('',#1889,#1867,#1181,.T.);
#2380=EDGE_CURVE('',#1892,#1868,#1182,.T.);
#2381=EDGE_CURVE('',#1886,#1861,#1183,.T.);
#2382=EDGE_CURVE('',#1887,#1862,#1184,.T.);
#2383=EDGE_CURVE('',#1885,#1863,#1185,.T.);
#2384=EDGE_CURVE('',#1888,#1864,#1186,.T.);
#2385=EDGE_CURVE('',#1882,#1857,#1187,.T.);
#2386=EDGE_CURVE('',#1883,#1858,#1188,.T.);
#2387=EDGE_CURVE('',#1881,#1859,#1189,.T.);
#2388=EDGE_CURVE('',#1884,#1860,#1190,.T.);
#2389=EDGE_CURVE('',#1878,#1853,#1191,.T.);
#2390=EDGE_CURVE('',#1879,#1854,#1192,.T.);
#2391=EDGE_CURVE('',#1877,#1855,#1193,.T.);
#2392=EDGE_CURVE('',#1880,#1856,#1194,.T.);
#2393=EDGE_CURVE('',#1901,#1901,#322,.T.);
#2394=EDGE_CURVE('',#1901,#1902,#1195,.T.);
#2395=EDGE_CURVE('',#1902,#1903,#323,.T.);
#2396=EDGE_CURVE('',#1903,#1904,#1196,.T.);
#2397=EDGE_CURVE('',#1904,#1905,#324,.T.);
#2398=EDGE_CURVE('',#1906,#1905,#1197,.T.);
#2399=EDGE_CURVE('',#1906,#1907,#325,.T.);
#2400=EDGE_CURVE('',#1907,#1908,#1198,.T.);
#2401=EDGE_CURVE('',#1908,#1909,#326,.T.);
#2402=EDGE_CURVE('',#1910,#1909,#1199,.T.);
#2403=EDGE_CURVE('',#1910,#1902,#327,.T.);
#2404=EDGE_CURVE('',#1908,#1911,#1200,.T.);
#2405=EDGE_CURVE('',#1911,#1912,#1201,.T.);
#2406=EDGE_CURVE('',#1912,#1905,#1202,.T.);
#2407=EDGE_CURVE('',#1904,#1913,#1203,.T.);
#2408=EDGE_CURVE('',#1913,#1914,#1204,.T.);
#2409=EDGE_CURVE('',#1914,#1909,#1205,.T.);
#2410=EDGE_CURVE('',#1915,#1915,#328,.T.);
#2411=EDGE_CURVE('',#1916,#1917,#1206,.T.);
#2412=EDGE_CURVE('',#1903,#1916,#1207,.T.);
#2413=EDGE_CURVE('',#1917,#1910,#1208,.T.);
#2414=EDGE_CURVE('',#1917,#1914,#1209,.T.);
#2415=EDGE_CURVE('',#1916,#1913,#1210,.T.);
#2416=EDGE_CURVE('',#1918,#1906,#1211,.T.);
#2417=EDGE_CURVE('',#1919,#1918,#1212,.T.);
#2418=EDGE_CURVE('',#1907,#1919,#1213,.T.);
#2419=EDGE_CURVE('',#1919,#1911,#1214,.T.);
#2420=EDGE_CURVE('',#1918,#1912,#1215,.T.);
#2421=EDGE_CURVE('',#1920,#1920,#329,.T.);
#2422=EDGE_CURVE('',#1920,#1915,#1216,.T.);
#2423=EDGE_CURVE('',#1921,#1922,#330,.F.);
#2424=EDGE_CURVE('',#1922,#1923,#331,.T.);
#2425=EDGE_CURVE('',#1923,#1924,#332,.T.);
#2426=EDGE_CURVE('',#1924,#1923,#333,.T.);
#2427=EDGE_CURVE('',#1922,#1921,#334,.F.);
#2428=EDGE_CURVE('',#1925,#1925,#335,.T.);
#2429=EDGE_CURVE('',#1925,#1924,#1217,.T.);
#2430=EDGE_CURVE('',#1926,#1927,#336,.T.);
#2431=EDGE_CURVE('',#1927,#1926,#337,.T.);
#2432=EDGE_CURVE('',#1927,#1928,#1218,.T.);
#2433=EDGE_CURVE('',#1928,#1928,#338,.T.);
#2434=EDGE_CURVE('',#1929,#1929,#339,.T.);
#2435=EDGE_CURVE('',#1930,#1930,#340,.T.);
#2436=EDGE_CURVE('',#1930,#1929,#341,.T.);
#2437=EDGE_CURVE('',#1931,#1931,#342,.T.);
#2438=EDGE_CURVE('',#1931,#1930,#1219,.T.);
#2439=EDGE_CURVE('',#1932,#1932,#343,.T.);
#2440=EDGE_CURVE('',#1932,#1931,#344,.T.);
#2441=EDGE_CURVE('',#1926,#1933,#345,.T.);
#2442=EDGE_CURVE('',#1933,#1934,#346,.F.);
#2443=EDGE_CURVE('',#1934,#1933,#347,.F.);
#2444=EDGE_CURVE('',#1921,#1935,#1220,.T.);
#2445=EDGE_CURVE('',#1935,#1935,#348,.T.);
#2446=EDGE_CURVE('',#1936,#1936,#349,.T.);
#2447=EDGE_CURVE('',#1936,#1934,#1221,.T.);
#2448=EDGE_CURVE('',#1937,#1937,#350,.T.);
#2449=EDGE_CURVE('',#1937,#1938,#351,.T.);
#2450=EDGE_CURVE('',#1938,#1938,#352,.T.);
#2451=EDGE_CURVE('',#1938,#1939,#1222,.T.);
#2452=EDGE_CURVE('',#1939,#1939,#353,.T.);
#2453=EDGE_CURVE('',#1939,#1940,#354,.T.);
#2454=EDGE_CURVE('',#1940,#1940,#355,.T.);
#2455=EDGE_CURVE('',#1941,#1941,#356,.T.);
#2456=EDGE_CURVE('',#1941,#1942,#1223,.T.);
#2457=EDGE_CURVE('',#1942,#1942,#357,.T.);
#2458=EDGE_CURVE('',#1943,#1944,#358,.T.);
#2459=EDGE_CURVE('',#1944,#1943,#359,.T.);
#2460=EDGE_CURVE('',#1943,#1945,#1224,.T.);
#2461=EDGE_CURVE('',#1945,#1945,#360,.T.);
#2462=EDGE_CURVE('',#1946,#1946,#361,.T.);
#2463=EDGE_CURVE('',#1946,#1947,#1225,.T.);
#2464=EDGE_CURVE('',#1947,#1947,#362,.T.);
#2465=EDGE_CURVE('',#1948,#1948,#363,.T.);
#2466=EDGE_CURVE('',#1948,#1949,#1226,.T.);
#2467=EDGE_CURVE('',#1949,#1949,#364,.T.);
#2468=EDGE_CURVE('',#1950,#1950,#365,.T.);
#2469=EDGE_CURVE('',#1950,#1951,#1227,.T.);
#2470=EDGE_CURVE('',#1951,#1951,#366,.T.);
#2471=EDGE_CURVE('',#1952,#1952,#367,.T.);
#2472=EDGE_CURVE('',#1952,#1953,#1228,.T.);
#2473=EDGE_CURVE('',#1953,#1953,#368,.T.);
#2474=EDGE_CURVE('',#1954,#1954,#369,.T.);
#2475=EDGE_CURVE('',#1954,#1955,#1229,.T.);
#2476=EDGE_CURVE('',#1955,#1955,#370,.T.);
#2477=EDGE_CURVE('',#1956,#1956,#371,.T.);
#2478=EDGE_CURVE('',#1956,#1957,#1230,.T.);
#2479=EDGE_CURVE('',#1957,#1957,#372,.T.);
#2480=EDGE_CURVE('',#1958,#1958,#373,.T.);
#2481=EDGE_CURVE('',#1958,#1959,#1231,.T.);
#2482=EDGE_CURVE('',#1959,#1959,#374,.T.);
#2483=EDGE_CURVE('',#1960,#1960,#375,.T.);
#2484=EDGE_CURVE('',#1961,#1961,#376,.T.);
#2485=EDGE_CURVE('',#1962,#1962,#377,.T.);
#2486=EDGE_CURVE('',#1963,#1963,#378,.F.);
#2487=EDGE_CURVE('',#1964,#1964,#379,.T.);
#2488=EDGE_CURVE('',#1964,#1963,#1232,.T.);
#2489=EDGE_CURVE('',#1965,#1965,#380,.T.);
#2490=EDGE_CURVE('',#1965,#1966,#1233,.T.);
#2491=EDGE_CURVE('',#1966,#1966,#381,.T.);
#2492=EDGE_CURVE('',#1961,#1967,#1234,.T.);
#2493=EDGE_CURVE('',#1967,#1967,#382,.T.);
#2494=EDGE_CURVE('',#1962,#1960,#1235,.T.);
#2495=EDGE_CURVE('',#1942,#1968,#1236,.T.);
#2496=EDGE_CURVE('',#1969,#1968,#383,.T.);
#2497=EDGE_CURVE('',#1968,#1969,#384,.T.);
#2498=EDGE_CURVE('',#1944,#1970,#1237,.T.);
#2499=EDGE_CURVE('',#1970,#1970,#385,.T.);
#2500=EDGE_CURVE('',#1970,#1969,#1238,.T.);
#2501=EDGE_CURVE('',#1971,#1972,#1239,.T.);
#2502=EDGE_CURVE('',#1971,#1973,#1240,.T.);
#2503=EDGE_CURVE('',#1973,#1974,#1241,.T.);
#2504=EDGE_CURVE('',#1972,#1974,#1242,.T.);
#2505=EDGE_CURVE('',#1975,#1976,#1243,.T.);
#2506=EDGE_CURVE('',#1975,#1971,#1244,.T.);
#2507=EDGE_CURVE('',#1976,#1972,#1245,.T.);
#2508=EDGE_CURVE('',#1977,#1978,#1246,.T.);
#2509=EDGE_CURVE('',#1977,#1975,#1247,.T.);
#2510=EDGE_CURVE('',#1978,#1976,#1248,.T.);
#2511=EDGE_CURVE('',#1979,#1971,#386,.T.);
#2512=EDGE_CURVE('',#1979,#1980,#1249,.T.);
#2513=EDGE_CURVE('',#1980,#1973,#387,.T.);
#2514=EDGE_CURVE('',#1981,#1975,#388,.T.);
#2515=EDGE_CURVE('',#1981,#1979,#1250,.T.);
#2516=EDGE_CURVE('',#1982,#1977,#389,.T.);
#2517=EDGE_CURVE('',#1982,#1981,#1251,.T.);
#2518=EDGE_CURVE('',#1973,#1977,#1252,.T.);
#2519=EDGE_CURVE('',#1980,#1982,#1253,.T.);
#2520=EDGE_CURVE('',#1983,#1979,#1254,.T.);
#2521=EDGE_CURVE('',#1983,#1984,#1255,.T.);
#2522=EDGE_CURVE('',#1984,#1980,#1256,.T.);
#2523=EDGE_CURVE('',#1985,#1981,#1257,.T.);
#2524=EDGE_CURVE('',#1985,#1983,#1258,.T.);
#2525=EDGE_CURVE('',#1986,#1982,#1259,.T.);
#2526=EDGE_CURVE('',#1986,#1985,#1260,.T.);
#2527=EDGE_CURVE('',#1984,#1986,#1261,.T.);
#2528=EDGE_CURVE('',#1972,#1983,#390,.T.);
#2529=EDGE_CURVE('',#1974,#1984,#391,.T.);
#2530=EDGE_CURVE('',#1976,#1985,#392,.T.);
#2531=EDGE_CURVE('',#1978,#1986,#393,.T.);
#2532=EDGE_CURVE('',#1974,#1978,#1262,.T.);
#2533=ORIENTED_EDGE('',*,*,#1987,.F.);
#2534=ORIENTED_EDGE('',*,*,#1988,.T.);
#2535=ORIENTED_EDGE('',*,*,#1989,.T.);
#2536=ORIENTED_EDGE('',*,*,#1990,.T.);
#2537=ORIENTED_EDGE('',*,*,#1991,.F.);
#2538=ORIENTED_EDGE('',*,*,#1992,.F.);
#2539=ORIENTED_EDGE('',*,*,#1993,.T.);
#2540=ORIENTED_EDGE('',*,*,#1994,.T.);
#2541=ORIENTED_EDGE('',*,*,#1995,.F.);
#2542=ORIENTED_EDGE('',*,*,#1996,.F.);
#2543=ORIENTED_EDGE('',*,*,#1997,.T.);
#2544=ORIENTED_EDGE('',*,*,#1998,.F.);
#2545=ORIENTED_EDGE('',*,*,#1999,.F.);
#2546=ORIENTED_EDGE('',*,*,#2000,.F.);
#2547=ORIENTED_EDGE('',*,*,#2001,.F.);
#2548=ORIENTED_EDGE('',*,*,#2002,.F.);
#2549=ORIENTED_EDGE('',*,*,#2003,.F.);
#2550=ORIENTED_EDGE('',*,*,#2004,.T.);
#2551=ORIENTED_EDGE('',*,*,#2005,.T.);
#2552=ORIENTED_EDGE('',*,*,#2006,.F.);
#2553=ORIENTED_EDGE('',*,*,#2007,.F.);
#2554=ORIENTED_EDGE('',*,*,#2008,.T.);
#2555=ORIENTED_EDGE('',*,*,#2009,.T.);
#2556=ORIENTED_EDGE('',*,*,#2010,.F.);
#2557=ORIENTED_EDGE('',*,*,#2011,.T.);
#2558=ORIENTED_EDGE('',*,*,#2012,.T.);
#2559=ORIENTED_EDGE('',*,*,#2013,.T.);
#2560=ORIENTED_EDGE('',*,*,#2014,.T.);
#2561=ORIENTED_EDGE('',*,*,#1992,.T.);
#2562=ORIENTED_EDGE('',*,*,#2015,.T.);
#2563=ORIENTED_EDGE('',*,*,#2016,.F.);
#2564=ORIENTED_EDGE('',*,*,#2017,.T.);
#2565=ORIENTED_EDGE('',*,*,#2018,.T.);
#2566=ORIENTED_EDGE('',*,*,#2019,.T.);
#2567=ORIENTED_EDGE('',*,*,#2020,.T.);
#2568=ORIENTED_EDGE('',*,*,#2016,.T.);
#2569=ORIENTED_EDGE('',*,*,#2021,.T.);
#2570=ORIENTED_EDGE('',*,*,#2022,.F.);
#2571=ORIENTED_EDGE('',*,*,#2023,.T.);
#2572=ORIENTED_EDGE('',*,*,#2024,.T.);
#2573=ORIENTED_EDGE('',*,*,#2025,.T.);
#2574=ORIENTED_EDGE('',*,*,#2026,.T.);
#2575=ORIENTED_EDGE('',*,*,#2027,.T.);
#2576=ORIENTED_EDGE('',*,*,#2028,.T.);
#2577=ORIENTED_EDGE('',*,*,#2029,.T.);
#2578=ORIENTED_EDGE('',*,*,#2030,.T.);
#2579=ORIENTED_EDGE('',*,*,#2031,.T.);
#2580=ORIENTED_EDGE('',*,*,#2022,.T.);
#2581=ORIENTED_EDGE('',*,*,#2032,.F.);
#2582=ORIENTED_EDGE('',*,*,#1990,.F.);
#2583=ORIENTED_EDGE('',*,*,#2033,.T.);
#2584=ORIENTED_EDGE('',*,*,#2034,.T.);
#2585=ORIENTED_EDGE('',*,*,#2035,.F.);
#2586=ORIENTED_EDGE('',*,*,#2036,.T.);
#2587=ORIENTED_EDGE('',*,*,#2037,.T.);
#2588=ORIENTED_EDGE('',*,*,#2038,.F.);
#2589=ORIENTED_EDGE('',*,*,#2039,.F.);
#2590=ORIENTED_EDGE('',*,*,#2040,.F.);
#2591=ORIENTED_EDGE('',*,*,#2041,.F.);
#2592=ORIENTED_EDGE('',*,*,#2042,.T.);
#2593=ORIENTED_EDGE('',*,*,#2043,.F.);
#2594=ORIENTED_EDGE('',*,*,#2044,.F.);
#2595=ORIENTED_EDGE('',*,*,#2045,.T.);
#2596=ORIENTED_EDGE('',*,*,#2046,.F.);
#2597=ORIENTED_EDGE('',*,*,#2047,.T.);
#2598=ORIENTED_EDGE('',*,*,#2048,.T.);
#2599=ORIENTED_EDGE('',*,*,#2049,.F.);
#2600=ORIENTED_EDGE('',*,*,#2050,.T.);
#2601=ORIENTED_EDGE('',*,*,#2051,.T.);
#2602=ORIENTED_EDGE('',*,*,#2052,.T.);
#2603=ORIENTED_EDGE('',*,*,#2053,.F.);
#2604=ORIENTED_EDGE('',*,*,#2054,.T.);
#2605=ORIENTED_EDGE('',*,*,#2055,.T.);
#2606=ORIENTED_EDGE('',*,*,#2056,.F.);
#2607=ORIENTED_EDGE('',*,*,#2057,.F.);
#2608=ORIENTED_EDGE('',*,*,#2058,.T.);
#2609=ORIENTED_EDGE('',*,*,#2059,.F.);
#2610=ORIENTED_EDGE('',*,*,#2060,.T.);
#2611=ORIENTED_EDGE('',*,*,#2061,.T.);
#2612=ORIENTED_EDGE('',*,*,#2062,.F.);
#2613=ORIENTED_EDGE('',*,*,#2063,.T.);
#2614=ORIENTED_EDGE('',*,*,#2064,.T.);
#2615=ORIENTED_EDGE('',*,*,#2065,.T.);
#2616=ORIENTED_EDGE('',*,*,#2066,.T.);
#2617=ORIENTED_EDGE('',*,*,#2067,.F.);
#2618=ORIENTED_EDGE('',*,*,#2068,.T.);
#2619=ORIENTED_EDGE('',*,*,#2069,.T.);
#2620=ORIENTED_EDGE('',*,*,#2070,.F.);
#2621=ORIENTED_EDGE('',*,*,#2071,.F.);
#2622=ORIENTED_EDGE('',*,*,#2072,.F.);
#2623=ORIENTED_EDGE('',*,*,#2073,.F.);
#2624=ORIENTED_EDGE('',*,*,#2074,.T.);
#2625=ORIENTED_EDGE('',*,*,#2075,.F.);
#2626=ORIENTED_EDGE('',*,*,#2076,.F.);
#2627=ORIENTED_EDGE('',*,*,#2077,.F.);
#2628=ORIENTED_EDGE('',*,*,#2049,.T.);
#2629=ORIENTED_EDGE('',*,*,#2078,.F.);
#2630=ORIENTED_EDGE('',*,*,#2079,.F.);
#2631=ORIENTED_EDGE('',*,*,#2053,.T.);
#2632=ORIENTED_EDGE('',*,*,#2080,.F.);
#2633=ORIENTED_EDGE('',*,*,#2081,.F.);
#2634=ORIENTED_EDGE('',*,*,#2082,.T.);
#2635=ORIENTED_EDGE('',*,*,#2083,.F.);
#2636=ORIENTED_EDGE('',*,*,#2084,.F.);
#2637=ORIENTED_EDGE('',*,*,#2085,.F.);
#2638=ORIENTED_EDGE('',*,*,#2086,.F.);
#2639=ORIENTED_EDGE('',*,*,#2057,.T.);
#2640=ORIENTED_EDGE('',*,*,#2087,.T.);
#2641=ORIENTED_EDGE('',*,*,#2015,.F.);
#2642=ORIENTED_EDGE('',*,*,#1991,.T.);
#2643=ORIENTED_EDGE('',*,*,#2032,.T.);
#2644=ORIENTED_EDGE('',*,*,#2021,.F.);
#2645=ORIENTED_EDGE('',*,*,#2088,.T.);
#2646=ORIENTED_EDGE('',*,*,#2089,.T.);
#2647=ORIENTED_EDGE('',*,*,#2090,.F.);
#2648=ORIENTED_EDGE('',*,*,#2040,.T.);
#2649=ORIENTED_EDGE('',*,*,#2091,.T.);
#2650=ORIENTED_EDGE('',*,*,#2092,.F.);
#2651=ORIENTED_EDGE('',*,*,#2054,.F.);
#2652=ORIENTED_EDGE('',*,*,#2079,.T.);
#2653=ORIENTED_EDGE('',*,*,#2093,.F.);
#2654=ORIENTED_EDGE('',*,*,#2094,.F.);
#2655=ORIENTED_EDGE('',*,*,#2095,.F.);
#2656=ORIENTED_EDGE('',*,*,#2096,.F.);
#2657=ORIENTED_EDGE('',*,*,#2097,.F.);
#2658=ORIENTED_EDGE('',*,*,#2043,.T.);
#2659=ORIENTED_EDGE('',*,*,#2098,.T.);
#2660=ORIENTED_EDGE('',*,*,#2099,.F.);
#2661=ORIENTED_EDGE('',*,*,#2091,.F.);
#2662=ORIENTED_EDGE('',*,*,#2039,.T.);
#2663=ORIENTED_EDGE('',*,*,#2100,.F.);
#2664=ORIENTED_EDGE('',*,*,#2101,.F.);
#2665=ORIENTED_EDGE('',*,*,#2102,.F.);
#2666=ORIENTED_EDGE('',*,*,#2072,.T.);
#2667=ORIENTED_EDGE('',*,*,#2042,.F.);
#2668=ORIENTED_EDGE('',*,*,#2103,.T.);
#2669=ORIENTED_EDGE('',*,*,#2104,.T.);
#2670=ORIENTED_EDGE('',*,*,#2105,.T.);
#2671=ORIENTED_EDGE('',*,*,#2087,.F.);
#2672=ORIENTED_EDGE('',*,*,#2056,.T.);
#2673=ORIENTED_EDGE('',*,*,#2106,.T.);
#2674=ORIENTED_EDGE('',*,*,#2098,.F.);
#2675=ORIENTED_EDGE('',*,*,#2092,.T.);
#2676=ORIENTED_EDGE('',*,*,#2099,.T.);
#2677=ORIENTED_EDGE('',*,*,#2106,.F.);
#2678=ORIENTED_EDGE('',*,*,#2055,.F.);
#2679=ORIENTED_EDGE('',*,*,#2107,.F.);
#2680=ORIENTED_EDGE('',*,*,#2108,.F.);
#2681=ORIENTED_EDGE('',*,*,#2077,.T.);
#2682=ORIENTED_EDGE('',*,*,#2109,.T.);
#2683=ORIENTED_EDGE('',*,*,#2110,.F.);
#2684=ORIENTED_EDGE('',*,*,#2111,.F.);
#2685=ORIENTED_EDGE('',*,*,#2112,.T.);
#2686=ORIENTED_EDGE('',*,*,#1996,.T.);
#2687=ORIENTED_EDGE('',*,*,#2113,.F.);
#2688=ORIENTED_EDGE('',*,*,#2050,.F.);
#2689=ORIENTED_EDGE('',*,*,#1995,.T.);
#2690=ORIENTED_EDGE('',*,*,#2114,.T.);
#2691=ORIENTED_EDGE('',*,*,#2115,.F.);
#2692=ORIENTED_EDGE('',*,*,#2051,.F.);
#2693=ORIENTED_EDGE('',*,*,#2113,.T.);
#2694=ORIENTED_EDGE('',*,*,#2115,.T.);
#2695=ORIENTED_EDGE('',*,*,#2116,.T.);
#2696=ORIENTED_EDGE('',*,*,#2117,.F.);
#2697=ORIENTED_EDGE('',*,*,#2118,.T.);
#2698=ORIENTED_EDGE('',*,*,#2119,.T.);
#2699=ORIENTED_EDGE('',*,*,#2120,.F.);
#2700=ORIENTED_EDGE('',*,*,#2121,.F.);
#2701=ORIENTED_EDGE('',*,*,#2080,.T.);
#2702=ORIENTED_EDGE('',*,*,#2052,.F.);
#2703=ORIENTED_EDGE('',*,*,#2122,.F.);
#2704=ORIENTED_EDGE('',*,*,#2123,.T.);
#2705=ORIENTED_EDGE('',*,*,#2124,.F.);
#2706=ORIENTED_EDGE('',*,*,#2058,.F.);
#2707=ORIENTED_EDGE('',*,*,#2086,.T.);
#2708=ORIENTED_EDGE('',*,*,#2125,.T.);
#2709=ORIENTED_EDGE('',*,*,#2126,.F.);
#2710=ORIENTED_EDGE('',*,*,#2127,.F.);
#2711=ORIENTED_EDGE('',*,*,#2128,.T.);
#2712=ORIENTED_EDGE('',*,*,#1987,.T.);
#2713=ORIENTED_EDGE('',*,*,#2129,.F.);
#2714=ORIENTED_EDGE('',*,*,#2047,.F.);
#2715=ORIENTED_EDGE('',*,*,#2124,.T.);
#2716=ORIENTED_EDGE('',*,*,#2130,.T.);
#2717=ORIENTED_EDGE('',*,*,#1998,.T.);
#2718=ORIENTED_EDGE('',*,*,#2131,.T.);
#2719=ORIENTED_EDGE('',*,*,#2132,.T.);
#2720=ORIENTED_EDGE('',*,*,#2133,.F.);
#2721=ORIENTED_EDGE('',*,*,#2134,.F.);
#2722=ORIENTED_EDGE('',*,*,#2075,.T.);
#2723=ORIENTED_EDGE('',*,*,#2048,.F.);
#2724=ORIENTED_EDGE('',*,*,#2129,.T.);
#2725=ORIENTED_EDGE('',*,*,#2073,.T.);
#2726=ORIENTED_EDGE('',*,*,#2102,.T.);
#2727=ORIENTED_EDGE('',*,*,#2135,.F.);
#2728=ORIENTED_EDGE('',*,*,#2028,.F.);
#2729=ORIENTED_EDGE('',*,*,#2136,.T.);
#2730=ORIENTED_EDGE('',*,*,#2137,.T.);
#2731=ORIENTED_EDGE('',*,*,#2138,.F.);
#2732=ORIENTED_EDGE('',*,*,#2139,.F.);
#2733=ORIENTED_EDGE('',*,*,#2101,.T.);
#2734=ORIENTED_EDGE('',*,*,#2140,.F.);
#2735=ORIENTED_EDGE('',*,*,#2141,.T.);
#2736=ORIENTED_EDGE('',*,*,#2018,.F.);
#2737=ORIENTED_EDGE('',*,*,#2135,.T.);
#2738=ORIENTED_EDGE('',*,*,#2142,.F.);
#2739=ORIENTED_EDGE('',*,*,#2143,.T.);
#2740=ORIENTED_EDGE('',*,*,#2140,.T.);
#2741=ORIENTED_EDGE('',*,*,#2100,.T.);
#2742=ORIENTED_EDGE('',*,*,#2038,.T.);
#2743=ORIENTED_EDGE('',*,*,#2144,.T.);
#2744=ORIENTED_EDGE('',*,*,#2145,.F.);
#2745=ORIENTED_EDGE('',*,*,#2146,.F.);
#2746=ORIENTED_EDGE('',*,*,#2147,.T.);
#2747=ORIENTED_EDGE('',*,*,#2071,.T.);
#2748=ORIENTED_EDGE('',*,*,#2148,.T.);
#2749=ORIENTED_EDGE('',*,*,#2149,.F.);
#2750=ORIENTED_EDGE('',*,*,#2150,.F.);
#2751=ORIENTED_EDGE('',*,*,#2151,.T.);
#2752=ORIENTED_EDGE('',*,*,#2026,.F.);
#2753=ORIENTED_EDGE('',*,*,#2152,.T.);
#2754=ORIENTED_EDGE('',*,*,#2095,.T.);
#2755=ORIENTED_EDGE('',*,*,#2153,.F.);
#2756=ORIENTED_EDGE('',*,*,#2154,.T.);
#2757=ORIENTED_EDGE('',*,*,#2155,.F.);
#2758=ORIENTED_EDGE('',*,*,#2156,.T.);
#2759=ORIENTED_EDGE('',*,*,#2157,.T.);
#2760=ORIENTED_EDGE('',*,*,#2158,.F.);
#2761=ORIENTED_EDGE('',*,*,#2159,.F.);
#2762=ORIENTED_EDGE('',*,*,#2044,.T.);
#2763=ORIENTED_EDGE('',*,*,#2097,.T.);
#2764=ORIENTED_EDGE('',*,*,#2096,.T.);
#2765=ORIENTED_EDGE('',*,*,#2152,.F.);
#2766=ORIENTED_EDGE('',*,*,#2025,.F.);
#2767=ORIENTED_EDGE('',*,*,#2160,.T.);
#2768=ORIENTED_EDGE('',*,*,#2153,.T.);
#2769=ORIENTED_EDGE('',*,*,#2067,.T.);
#2770=ORIENTED_EDGE('',*,*,#2161,.T.);
#2771=ORIENTED_EDGE('',*,*,#2004,.F.);
#2772=ORIENTED_EDGE('',*,*,#2162,.F.);
#2773=ORIENTED_EDGE('',*,*,#2070,.T.);
#2774=ORIENTED_EDGE('',*,*,#2163,.T.);
#2775=ORIENTED_EDGE('',*,*,#2005,.F.);
#2776=ORIENTED_EDGE('',*,*,#2161,.F.);
#2777=ORIENTED_EDGE('',*,*,#2164,.T.);
#2778=ORIENTED_EDGE('',*,*,#2006,.T.);
#2779=ORIENTED_EDGE('',*,*,#2163,.F.);
#2780=ORIENTED_EDGE('',*,*,#2069,.F.);
#2781=ORIENTED_EDGE('',*,*,#2162,.T.);
#2782=ORIENTED_EDGE('',*,*,#2003,.T.);
#2783=ORIENTED_EDGE('',*,*,#2164,.F.);
#2784=ORIENTED_EDGE('',*,*,#2068,.F.);
#2785=ORIENTED_EDGE('',*,*,#2059,.T.);
#2786=ORIENTED_EDGE('',*,*,#2165,.T.);
#2787=ORIENTED_EDGE('',*,*,#2008,.F.);
#2788=ORIENTED_EDGE('',*,*,#2166,.F.);
#2789=ORIENTED_EDGE('',*,*,#2062,.T.);
#2790=ORIENTED_EDGE('',*,*,#2167,.T.);
#2791=ORIENTED_EDGE('',*,*,#2009,.F.);
#2792=ORIENTED_EDGE('',*,*,#2165,.F.);
#2793=ORIENTED_EDGE('',*,*,#2168,.T.);
#2794=ORIENTED_EDGE('',*,*,#2010,.T.);
#2795=ORIENTED_EDGE('',*,*,#2167,.F.);
#2796=ORIENTED_EDGE('',*,*,#2061,.F.);
#2797=ORIENTED_EDGE('',*,*,#2166,.T.);
#2798=ORIENTED_EDGE('',*,*,#2007,.T.);
#2799=ORIENTED_EDGE('',*,*,#2168,.F.);
#2800=ORIENTED_EDGE('',*,*,#2060,.F.);
#2801=ORIENTED_EDGE('',*,*,#2066,.F.);
#2802=ORIENTED_EDGE('',*,*,#2169,.T.);
#2803=ORIENTED_EDGE('',*,*,#2002,.T.);
#2804=ORIENTED_EDGE('',*,*,#2169,.F.);
#2805=ORIENTED_EDGE('',*,*,#2065,.F.);
#2806=ORIENTED_EDGE('',*,*,#2170,.T.);
#2807=ORIENTED_EDGE('',*,*,#2001,.T.);
#2808=ORIENTED_EDGE('',*,*,#2170,.F.);
#2809=ORIENTED_EDGE('',*,*,#2064,.F.);
#2810=ORIENTED_EDGE('',*,*,#2171,.T.);
#2811=ORIENTED_EDGE('',*,*,#2000,.T.);
#2812=ORIENTED_EDGE('',*,*,#2171,.F.);
#2813=ORIENTED_EDGE('',*,*,#2063,.F.);
#2814=ORIENTED_EDGE('',*,*,#2172,.T.);
#2815=ORIENTED_EDGE('',*,*,#1999,.T.);
#2816=ORIENTED_EDGE('',*,*,#2172,.F.);
#2817=ORIENTED_EDGE('',*,*,#2173,.F.);
#2818=ORIENTED_EDGE('',*,*,#2174,.T.);
#2819=ORIENTED_EDGE('',*,*,#2175,.F.);
#2820=ORIENTED_EDGE('',*,*,#2176,.T.);
#2821=ORIENTED_EDGE('',*,*,#2177,.T.);
#2822=ORIENTED_EDGE('',*,*,#2178,.F.);
#2823=ORIENTED_EDGE('',*,*,#2179,.F.);
#2824=ORIENTED_EDGE('',*,*,#2083,.T.);
#2825=ORIENTED_EDGE('',*,*,#2105,.F.);
#2826=ORIENTED_EDGE('',*,*,#2180,.F.);
#2827=ORIENTED_EDGE('',*,*,#2181,.T.);
#2828=ORIENTED_EDGE('',*,*,#2029,.F.);
#2829=ORIENTED_EDGE('',*,*,#2182,.T.);
#2830=ORIENTED_EDGE('',*,*,#2173,.T.);
#2831=ORIENTED_EDGE('',*,*,#2104,.F.);
#2832=ORIENTED_EDGE('',*,*,#2183,.F.);
#2833=ORIENTED_EDGE('',*,*,#2184,.T.);
#2834=ORIENTED_EDGE('',*,*,#2180,.T.);
#2835=ORIENTED_EDGE('',*,*,#2103,.F.);
#2836=ORIENTED_EDGE('',*,*,#2041,.T.);
#2837=ORIENTED_EDGE('',*,*,#2185,.T.);
#2838=ORIENTED_EDGE('',*,*,#2186,.F.);
#2839=ORIENTED_EDGE('',*,*,#2187,.F.);
#2840=ORIENTED_EDGE('',*,*,#2188,.T.);
#2841=ORIENTED_EDGE('',*,*,#2189,.T.);
#2842=ORIENTED_EDGE('',*,*,#2190,.T.);
#2843=ORIENTED_EDGE('',*,*,#2191,.F.);
#2844=ORIENTED_EDGE('',*,*,#2192,.T.);
#2845=ORIENTED_EDGE('',*,*,#2193,.T.);
#2846=ORIENTED_EDGE('',*,*,#2194,.F.);
#2847=ORIENTED_EDGE('',*,*,#2195,.F.);
#2848=ORIENTED_EDGE('',*,*,#2035,.T.);
#2849=ORIENTED_EDGE('',*,*,#2090,.T.);
#2850=ORIENTED_EDGE('',*,*,#2189,.F.);
#2851=ORIENTED_EDGE('',*,*,#2094,.T.);
#2852=ORIENTED_EDGE('',*,*,#2196,.T.);
#2853=ORIENTED_EDGE('',*,*,#2197,.T.);
#2854=ORIENTED_EDGE('',*,*,#2012,.F.);
#2855=ORIENTED_EDGE('',*,*,#2198,.T.);
#2856=ORIENTED_EDGE('',*,*,#2199,.F.);
#2857=ORIENTED_EDGE('',*,*,#2200,.T.);
#2858=ORIENTED_EDGE('',*,*,#2196,.F.);
#2859=ORIENTED_EDGE('',*,*,#2093,.T.);
#2860=ORIENTED_EDGE('',*,*,#2078,.T.);
#2861=ORIENTED_EDGE('',*,*,#2201,.T.);
#2862=ORIENTED_EDGE('',*,*,#2202,.F.);
#2863=ORIENTED_EDGE('',*,*,#2203,.F.);
#2864=ORIENTED_EDGE('',*,*,#2204,.T.);
#2865=ORIENTED_EDGE('',*,*,#2119,.F.);
#2866=ORIENTED_EDGE('',*,*,#2205,.T.);
#2867=ORIENTED_EDGE('',*,*,#2206,.T.);
#2868=ORIENTED_EDGE('',*,*,#2207,.F.);
#2869=ORIENTED_EDGE('',*,*,#2208,.F.);
#2870=ORIENTED_EDGE('',*,*,#2081,.T.);
#2871=ORIENTED_EDGE('',*,*,#2121,.T.);
#2872=ORIENTED_EDGE('',*,*,#2209,.F.);
#2873=ORIENTED_EDGE('',*,*,#2201,.F.);
#2874=ORIENTED_EDGE('',*,*,#2082,.F.);
#2875=ORIENTED_EDGE('',*,*,#2208,.T.);
#2876=ORIENTED_EDGE('',*,*,#2210,.F.);
#2877=ORIENTED_EDGE('',*,*,#2206,.F.);
#2878=ORIENTED_EDGE('',*,*,#2211,.T.);
#2879=ORIENTED_EDGE('',*,*,#2203,.T.);
#2880=ORIENTED_EDGE('',*,*,#2212,.F.);
#2881=ORIENTED_EDGE('',*,*,#2213,.T.);
#2882=ORIENTED_EDGE('',*,*,#2214,.T.);
#2883=ORIENTED_EDGE('',*,*,#2215,.T.);
#2884=ORIENTED_EDGE('',*,*,#2216,.T.);
#2885=ORIENTED_EDGE('',*,*,#2217,.T.);
#2886=ORIENTED_EDGE('',*,*,#2218,.T.);
#2887=ORIENTED_EDGE('',*,*,#2207,.T.);
#2888=ORIENTED_EDGE('',*,*,#2212,.T.);
#2889=ORIENTED_EDGE('',*,*,#2202,.T.);
#2890=ORIENTED_EDGE('',*,*,#2210,.T.);
#2891=ORIENTED_EDGE('',*,*,#2209,.T.);
#2892=ORIENTED_EDGE('',*,*,#2120,.T.);
#2893=ORIENTED_EDGE('',*,*,#2144,.F.);
#2894=ORIENTED_EDGE('',*,*,#2037,.F.);
#2895=ORIENTED_EDGE('',*,*,#2219,.T.);
#2896=ORIENTED_EDGE('',*,*,#2220,.F.);
#2897=ORIENTED_EDGE('',*,*,#2221,.F.);
#2898=ORIENTED_EDGE('',*,*,#2222,.T.);
#2899=ORIENTED_EDGE('',*,*,#2146,.T.);
#2900=ORIENTED_EDGE('',*,*,#2223,.F.);
#2901=ORIENTED_EDGE('',*,*,#2193,.F.);
#2902=ORIENTED_EDGE('',*,*,#2224,.T.);
#2903=ORIENTED_EDGE('',*,*,#2221,.T.);
#2904=ORIENTED_EDGE('',*,*,#2225,.F.);
#2905=ORIENTED_EDGE('',*,*,#2219,.F.);
#2906=ORIENTED_EDGE('',*,*,#2036,.F.);
#2907=ORIENTED_EDGE('',*,*,#2195,.T.);
#2908=ORIENTED_EDGE('',*,*,#2226,.F.);
#2909=ORIENTED_EDGE('',*,*,#2227,.T.);
#2910=ORIENTED_EDGE('',*,*,#2228,.T.);
#2911=ORIENTED_EDGE('',*,*,#2229,.T.);
#2912=ORIENTED_EDGE('',*,*,#2230,.T.);
#2913=ORIENTED_EDGE('',*,*,#2231,.T.);
#2914=ORIENTED_EDGE('',*,*,#2232,.T.);
#2915=ORIENTED_EDGE('',*,*,#2220,.T.);
#2916=ORIENTED_EDGE('',*,*,#2226,.T.);
#2917=ORIENTED_EDGE('',*,*,#2194,.T.);
#2918=ORIENTED_EDGE('',*,*,#2225,.T.);
#2919=ORIENTED_EDGE('',*,*,#2223,.T.);
#2920=ORIENTED_EDGE('',*,*,#2145,.T.);
#2921=ORIENTED_EDGE('',*,*,#2185,.F.);
#2922=ORIENTED_EDGE('',*,*,#2046,.T.);
#2923=ORIENTED_EDGE('',*,*,#2233,.T.);
#2924=ORIENTED_EDGE('',*,*,#2234,.F.);
#2925=ORIENTED_EDGE('',*,*,#2235,.F.);
#2926=ORIENTED_EDGE('',*,*,#2236,.T.);
#2927=ORIENTED_EDGE('',*,*,#2187,.T.);
#2928=ORIENTED_EDGE('',*,*,#2237,.F.);
#2929=ORIENTED_EDGE('',*,*,#2157,.F.);
#2930=ORIENTED_EDGE('',*,*,#2238,.T.);
#2931=ORIENTED_EDGE('',*,*,#2235,.T.);
#2932=ORIENTED_EDGE('',*,*,#2239,.F.);
#2933=ORIENTED_EDGE('',*,*,#2233,.F.);
#2934=ORIENTED_EDGE('',*,*,#2045,.F.);
#2935=ORIENTED_EDGE('',*,*,#2159,.T.);
#2936=ORIENTED_EDGE('',*,*,#2240,.F.);
#2937=ORIENTED_EDGE('',*,*,#2241,.T.);
#2938=ORIENTED_EDGE('',*,*,#2242,.T.);
#2939=ORIENTED_EDGE('',*,*,#2243,.T.);
#2940=ORIENTED_EDGE('',*,*,#2244,.T.);
#2941=ORIENTED_EDGE('',*,*,#2245,.T.);
#2942=ORIENTED_EDGE('',*,*,#2246,.T.);
#2943=ORIENTED_EDGE('',*,*,#2234,.T.);
#2944=ORIENTED_EDGE('',*,*,#2240,.T.);
#2945=ORIENTED_EDGE('',*,*,#2158,.T.);
#2946=ORIENTED_EDGE('',*,*,#2239,.T.);
#2947=ORIENTED_EDGE('',*,*,#2237,.T.);
#2948=ORIENTED_EDGE('',*,*,#2186,.T.);
#2949=ORIENTED_EDGE('',*,*,#2125,.F.);
#2950=ORIENTED_EDGE('',*,*,#2085,.T.);
#2951=ORIENTED_EDGE('',*,*,#2247,.T.);
#2952=ORIENTED_EDGE('',*,*,#2248,.F.);
#2953=ORIENTED_EDGE('',*,*,#2249,.F.);
#2954=ORIENTED_EDGE('',*,*,#2250,.T.);
#2955=ORIENTED_EDGE('',*,*,#2127,.T.);
#2956=ORIENTED_EDGE('',*,*,#2251,.F.);
#2957=ORIENTED_EDGE('',*,*,#2177,.F.);
#2958=ORIENTED_EDGE('',*,*,#2252,.T.);
#2959=ORIENTED_EDGE('',*,*,#2249,.T.);
#2960=ORIENTED_EDGE('',*,*,#2253,.F.);
#2961=ORIENTED_EDGE('',*,*,#2247,.F.);
#2962=ORIENTED_EDGE('',*,*,#2084,.T.);
#2963=ORIENTED_EDGE('',*,*,#2179,.T.);
#2964=ORIENTED_EDGE('',*,*,#2254,.F.);
#2965=ORIENTED_EDGE('',*,*,#2255,.T.);
#2966=ORIENTED_EDGE('',*,*,#2256,.T.);
#2967=ORIENTED_EDGE('',*,*,#2257,.T.);
#2968=ORIENTED_EDGE('',*,*,#2258,.T.);
#2969=ORIENTED_EDGE('',*,*,#2259,.T.);
#2970=ORIENTED_EDGE('',*,*,#2260,.T.);
#2971=ORIENTED_EDGE('',*,*,#2248,.T.);
#2972=ORIENTED_EDGE('',*,*,#2254,.T.);
#2973=ORIENTED_EDGE('',*,*,#2178,.T.);
#2974=ORIENTED_EDGE('',*,*,#2253,.T.);
#2975=ORIENTED_EDGE('',*,*,#2251,.T.);
#2976=ORIENTED_EDGE('',*,*,#2126,.T.);
#2977=ORIENTED_EDGE('',*,*,#2074,.F.);
#2978=ORIENTED_EDGE('',*,*,#2139,.T.);
#2979=ORIENTED_EDGE('',*,*,#2261,.F.);
#2980=ORIENTED_EDGE('',*,*,#2148,.F.);
#2981=ORIENTED_EDGE('',*,*,#2150,.T.);
#2982=ORIENTED_EDGE('',*,*,#2262,.F.);
#2983=ORIENTED_EDGE('',*,*,#2137,.F.);
#2984=ORIENTED_EDGE('',*,*,#2263,.T.);
#2985=ORIENTED_EDGE('',*,*,#2136,.F.);
#2986=ORIENTED_EDGE('',*,*,#2027,.F.);
#2987=ORIENTED_EDGE('',*,*,#2151,.F.);
#2988=ORIENTED_EDGE('',*,*,#2263,.F.);
#2989=ORIENTED_EDGE('',*,*,#2138,.T.);
#2990=ORIENTED_EDGE('',*,*,#2262,.T.);
#2991=ORIENTED_EDGE('',*,*,#2149,.T.);
#2992=ORIENTED_EDGE('',*,*,#2261,.T.);
#2993=ORIENTED_EDGE('',*,*,#2111,.T.);
#2994=ORIENTED_EDGE('',*,*,#2264,.F.);
#2995=ORIENTED_EDGE('',*,*,#2132,.F.);
#2996=ORIENTED_EDGE('',*,*,#2265,.T.);
#2997=ORIENTED_EDGE('',*,*,#2109,.F.);
#2998=ORIENTED_EDGE('',*,*,#2076,.T.);
#2999=ORIENTED_EDGE('',*,*,#2134,.T.);
#3000=ORIENTED_EDGE('',*,*,#2266,.F.);
#3001=ORIENTED_EDGE('',*,*,#2112,.F.);
#3002=ORIENTED_EDGE('',*,*,#2265,.F.);
#3003=ORIENTED_EDGE('',*,*,#2131,.F.);
#3004=ORIENTED_EDGE('',*,*,#1997,.F.);
#3005=ORIENTED_EDGE('',*,*,#2110,.T.);
#3006=ORIENTED_EDGE('',*,*,#2266,.T.);
#3007=ORIENTED_EDGE('',*,*,#2133,.T.);
#3008=ORIENTED_EDGE('',*,*,#2264,.T.);
#3009=ORIENTED_EDGE('',*,*,#2267,.F.);
#3010=ORIENTED_EDGE('',*,*,#2147,.F.);
#3011=ORIENTED_EDGE('',*,*,#2268,.F.);
#3012=ORIENTED_EDGE('',*,*,#2230,.F.);
#3013=ORIENTED_EDGE('',*,*,#2141,.F.);
#3014=ORIENTED_EDGE('',*,*,#2143,.F.);
#3015=ORIENTED_EDGE('',*,*,#2269,.F.);
#3016=ORIENTED_EDGE('',*,*,#2019,.F.);
#3017=ORIENTED_EDGE('',*,*,#2268,.T.);
#3018=ORIENTED_EDGE('',*,*,#2222,.F.);
#3019=ORIENTED_EDGE('',*,*,#2270,.F.);
#3020=ORIENTED_EDGE('',*,*,#2231,.F.);
#3021=ORIENTED_EDGE('',*,*,#2142,.T.);
#3022=ORIENTED_EDGE('',*,*,#2267,.T.);
#3023=ORIENTED_EDGE('',*,*,#2271,.F.);
#3024=ORIENTED_EDGE('',*,*,#2269,.T.);
#3025=ORIENTED_EDGE('',*,*,#2270,.T.);
#3026=ORIENTED_EDGE('',*,*,#2224,.F.);
#3027=ORIENTED_EDGE('',*,*,#2272,.F.);
#3028=ORIENTED_EDGE('',*,*,#2232,.F.);
#3029=ORIENTED_EDGE('',*,*,#2271,.T.);
#3030=ORIENTED_EDGE('',*,*,#2229,.F.);
#3031=ORIENTED_EDGE('',*,*,#2273,.F.);
#3032=ORIENTED_EDGE('',*,*,#2020,.F.);
#3033=ORIENTED_EDGE('',*,*,#2272,.T.);
#3034=ORIENTED_EDGE('',*,*,#2192,.F.);
#3035=ORIENTED_EDGE('',*,*,#2274,.F.);
#3036=ORIENTED_EDGE('',*,*,#2227,.F.);
#3037=ORIENTED_EDGE('',*,*,#2273,.T.);
#3038=ORIENTED_EDGE('',*,*,#2228,.F.);
#3039=ORIENTED_EDGE('',*,*,#2275,.F.);
#3040=ORIENTED_EDGE('',*,*,#2017,.F.);
#3041=ORIENTED_EDGE('',*,*,#2274,.T.);
#3042=ORIENTED_EDGE('',*,*,#2191,.T.);
#3043=ORIENTED_EDGE('',*,*,#2276,.F.);
#3044=ORIENTED_EDGE('',*,*,#2275,.T.);
#3045=ORIENTED_EDGE('',*,*,#2276,.T.);
#3046=ORIENTED_EDGE('',*,*,#2190,.F.);
#3047=ORIENTED_EDGE('',*,*,#2198,.F.);
#3048=ORIENTED_EDGE('',*,*,#2011,.F.);
#3049=ORIENTED_EDGE('',*,*,#2277,.F.);
#3050=ORIENTED_EDGE('',*,*,#2188,.F.);
#3051=ORIENTED_EDGE('',*,*,#2278,.F.);
#3052=ORIENTED_EDGE('',*,*,#2244,.F.);
#3053=ORIENTED_EDGE('',*,*,#2181,.F.);
#3054=ORIENTED_EDGE('',*,*,#2184,.F.);
#3055=ORIENTED_EDGE('',*,*,#2279,.F.);
#3056=ORIENTED_EDGE('',*,*,#2030,.F.);
#3057=ORIENTED_EDGE('',*,*,#2278,.T.);
#3058=ORIENTED_EDGE('',*,*,#2236,.F.);
#3059=ORIENTED_EDGE('',*,*,#2280,.F.);
#3060=ORIENTED_EDGE('',*,*,#2245,.F.);
#3061=ORIENTED_EDGE('',*,*,#2183,.T.);
#3062=ORIENTED_EDGE('',*,*,#2277,.T.);
#3063=ORIENTED_EDGE('',*,*,#2281,.F.);
#3064=ORIENTED_EDGE('',*,*,#2279,.T.);
#3065=ORIENTED_EDGE('',*,*,#2280,.T.);
#3066=ORIENTED_EDGE('',*,*,#2238,.F.);
#3067=ORIENTED_EDGE('',*,*,#2282,.F.);
#3068=ORIENTED_EDGE('',*,*,#2246,.F.);
#3069=ORIENTED_EDGE('',*,*,#2281,.T.);
#3070=ORIENTED_EDGE('',*,*,#2243,.F.);
#3071=ORIENTED_EDGE('',*,*,#2283,.F.);
#3072=ORIENTED_EDGE('',*,*,#2031,.F.);
#3073=ORIENTED_EDGE('',*,*,#2282,.T.);
#3074=ORIENTED_EDGE('',*,*,#2156,.F.);
#3075=ORIENTED_EDGE('',*,*,#2284,.F.);
#3076=ORIENTED_EDGE('',*,*,#2241,.F.);
#3077=ORIENTED_EDGE('',*,*,#2283,.T.);
#3078=ORIENTED_EDGE('',*,*,#2242,.F.);
#3079=ORIENTED_EDGE('',*,*,#2285,.F.);
#3080=ORIENTED_EDGE('',*,*,#2023,.F.);
#3081=ORIENTED_EDGE('',*,*,#2284,.T.);
#3082=ORIENTED_EDGE('',*,*,#2155,.T.);
#3083=ORIENTED_EDGE('',*,*,#2286,.F.);
#3084=ORIENTED_EDGE('',*,*,#2285,.T.);
#3085=ORIENTED_EDGE('',*,*,#2286,.T.);
#3086=ORIENTED_EDGE('',*,*,#2154,.F.);
#3087=ORIENTED_EDGE('',*,*,#2160,.F.);
#3088=ORIENTED_EDGE('',*,*,#2024,.F.);
#3089=ORIENTED_EDGE('',*,*,#2287,.F.);
#3090=ORIENTED_EDGE('',*,*,#2128,.F.);
#3091=ORIENTED_EDGE('',*,*,#2288,.F.);
#3092=ORIENTED_EDGE('',*,*,#2258,.F.);
#3093=ORIENTED_EDGE('',*,*,#2130,.F.);
#3094=ORIENTED_EDGE('',*,*,#2123,.F.);
#3095=ORIENTED_EDGE('',*,*,#2289,.F.);
#3096=ORIENTED_EDGE('',*,*,#1988,.F.);
#3097=ORIENTED_EDGE('',*,*,#2288,.T.);
#3098=ORIENTED_EDGE('',*,*,#2250,.F.);
#3099=ORIENTED_EDGE('',*,*,#2290,.F.);
#3100=ORIENTED_EDGE('',*,*,#2259,.F.);
#3101=ORIENTED_EDGE('',*,*,#2122,.T.);
#3102=ORIENTED_EDGE('',*,*,#2287,.T.);
#3103=ORIENTED_EDGE('',*,*,#2291,.F.);
#3104=ORIENTED_EDGE('',*,*,#2289,.T.);
#3105=ORIENTED_EDGE('',*,*,#2290,.T.);
#3106=ORIENTED_EDGE('',*,*,#2252,.F.);
#3107=ORIENTED_EDGE('',*,*,#2292,.F.);
#3108=ORIENTED_EDGE('',*,*,#2260,.F.);
#3109=ORIENTED_EDGE('',*,*,#2291,.T.);
#3110=ORIENTED_EDGE('',*,*,#2257,.F.);
#3111=ORIENTED_EDGE('',*,*,#2293,.F.);
#3112=ORIENTED_EDGE('',*,*,#1989,.F.);
#3113=ORIENTED_EDGE('',*,*,#2292,.T.);
#3114=ORIENTED_EDGE('',*,*,#2176,.F.);
#3115=ORIENTED_EDGE('',*,*,#2294,.F.);
#3116=ORIENTED_EDGE('',*,*,#2255,.F.);
#3117=ORIENTED_EDGE('',*,*,#2293,.T.);
#3118=ORIENTED_EDGE('',*,*,#2256,.F.);
#3119=ORIENTED_EDGE('',*,*,#2295,.F.);
#3120=ORIENTED_EDGE('',*,*,#2033,.F.);
#3121=ORIENTED_EDGE('',*,*,#2294,.T.);
#3122=ORIENTED_EDGE('',*,*,#2175,.T.);
#3123=ORIENTED_EDGE('',*,*,#2296,.F.);
#3124=ORIENTED_EDGE('',*,*,#2295,.T.);
#3125=ORIENTED_EDGE('',*,*,#2296,.T.);
#3126=ORIENTED_EDGE('',*,*,#2174,.F.);
#3127=ORIENTED_EDGE('',*,*,#2182,.F.);
#3128=ORIENTED_EDGE('',*,*,#2034,.F.);
#3129=ORIENTED_EDGE('',*,*,#2114,.F.);
#3130=ORIENTED_EDGE('',*,*,#1994,.F.);
#3131=ORIENTED_EDGE('',*,*,#2297,.F.);
#3132=ORIENTED_EDGE('',*,*,#2116,.F.);
#3133=ORIENTED_EDGE('',*,*,#2298,.F.);
#3134=ORIENTED_EDGE('',*,*,#2118,.F.);
#3135=ORIENTED_EDGE('',*,*,#2299,.F.);
#3136=ORIENTED_EDGE('',*,*,#2216,.F.);
#3137=ORIENTED_EDGE('',*,*,#2117,.T.);
#3138=ORIENTED_EDGE('',*,*,#2297,.T.);
#3139=ORIENTED_EDGE('',*,*,#2300,.F.);
#3140=ORIENTED_EDGE('',*,*,#2299,.T.);
#3141=ORIENTED_EDGE('',*,*,#2298,.T.);
#3142=ORIENTED_EDGE('',*,*,#2215,.F.);
#3143=ORIENTED_EDGE('',*,*,#2301,.F.);
#3144=ORIENTED_EDGE('',*,*,#2205,.F.);
#3145=ORIENTED_EDGE('',*,*,#2300,.T.);
#3146=ORIENTED_EDGE('',*,*,#1993,.F.);
#3147=ORIENTED_EDGE('',*,*,#2302,.F.);
#3148=ORIENTED_EDGE('',*,*,#2217,.F.);
#3149=ORIENTED_EDGE('',*,*,#2301,.T.);
#3150=ORIENTED_EDGE('',*,*,#2214,.F.);
#3151=ORIENTED_EDGE('',*,*,#2303,.F.);
#3152=ORIENTED_EDGE('',*,*,#2211,.F.);
#3153=ORIENTED_EDGE('',*,*,#2302,.T.);
#3154=ORIENTED_EDGE('',*,*,#2014,.F.);
#3155=ORIENTED_EDGE('',*,*,#2304,.F.);
#3156=ORIENTED_EDGE('',*,*,#2218,.F.);
#3157=ORIENTED_EDGE('',*,*,#2303,.T.);
#3158=ORIENTED_EDGE('',*,*,#2213,.F.);
#3159=ORIENTED_EDGE('',*,*,#2305,.F.);
#3160=ORIENTED_EDGE('',*,*,#2204,.F.);
#3161=ORIENTED_EDGE('',*,*,#2305,.T.);
#3162=ORIENTED_EDGE('',*,*,#2304,.T.);
#3163=ORIENTED_EDGE('',*,*,#2306,.F.);
#3164=ORIENTED_EDGE('',*,*,#2199,.T.);
#3165=ORIENTED_EDGE('',*,*,#2197,.F.);
#3166=ORIENTED_EDGE('',*,*,#2200,.F.);
#3167=ORIENTED_EDGE('',*,*,#2306,.T.);
#3168=ORIENTED_EDGE('',*,*,#2013,.F.);
#3169=ORIENTED_EDGE('',*,*,#2089,.F.);
#3170=ORIENTED_EDGE('',*,*,#2307,.T.);
#3171=ORIENTED_EDGE('',*,*,#2108,.T.);
#3172=ORIENTED_EDGE('',*,*,#2307,.F.);
#3173=ORIENTED_EDGE('',*,*,#2088,.F.);
#3174=ORIENTED_EDGE('',*,*,#2308,.T.);
#3175=ORIENTED_EDGE('',*,*,#2107,.T.);
#3176=ORIENTED_EDGE('',*,*,#2308,.F.);
#3177=ORIENTED_EDGE('',*,*,#2309,.T.);
#3178=ORIENTED_EDGE('',*,*,#2310,.F.);
#3179=ORIENTED_EDGE('',*,*,#2311,.F.);
#3180=ORIENTED_EDGE('',*,*,#2312,.T.);
#3181=ORIENTED_EDGE('',*,*,#2313,.T.);
#3182=ORIENTED_EDGE('',*,*,#2314,.F.);
#3183=ORIENTED_EDGE('',*,*,#2315,.F.);
#3184=ORIENTED_EDGE('',*,*,#2310,.T.);
#3185=ORIENTED_EDGE('',*,*,#2316,.F.);
#3186=ORIENTED_EDGE('',*,*,#2317,.F.);
#3187=ORIENTED_EDGE('',*,*,#2318,.T.);
#3188=ORIENTED_EDGE('',*,*,#2314,.T.);
#3189=ORIENTED_EDGE('',*,*,#2319,.F.);
#3190=ORIENTED_EDGE('',*,*,#2312,.F.);
#3191=ORIENTED_EDGE('',*,*,#2320,.T.);
#3192=ORIENTED_EDGE('',*,*,#2317,.T.);
#3193=ORIENTED_EDGE('',*,*,#2311,.T.);
#3194=ORIENTED_EDGE('',*,*,#2315,.T.);
#3195=ORIENTED_EDGE('',*,*,#2318,.F.);
#3196=ORIENTED_EDGE('',*,*,#2320,.F.);
#3197=ORIENTED_EDGE('',*,*,#2321,.F.);
#3198=ORIENTED_EDGE('',*,*,#2322,.F.);
#3199=ORIENTED_EDGE('',*,*,#2323,.F.);
#3200=ORIENTED_EDGE('',*,*,#2324,.F.);
#3201=ORIENTED_EDGE('',*,*,#2325,.F.);
#3202=ORIENTED_EDGE('',*,*,#2326,.F.);
#3203=ORIENTED_EDGE('',*,*,#2327,.F.);
#3204=ORIENTED_EDGE('',*,*,#2328,.F.);
#3205=ORIENTED_EDGE('',*,*,#2329,.F.);
#3206=ORIENTED_EDGE('',*,*,#2330,.F.);
#3207=ORIENTED_EDGE('',*,*,#2331,.F.);
#3208=ORIENTED_EDGE('',*,*,#2332,.F.);
#3209=ORIENTED_EDGE('',*,*,#2333,.F.);
#3210=ORIENTED_EDGE('',*,*,#2334,.F.);
#3211=ORIENTED_EDGE('',*,*,#2335,.F.);
#3212=ORIENTED_EDGE('',*,*,#2336,.F.);
#3213=ORIENTED_EDGE('',*,*,#2337,.F.);
#3214=ORIENTED_EDGE('',*,*,#2338,.F.);
#3215=ORIENTED_EDGE('',*,*,#2339,.F.);
#3216=ORIENTED_EDGE('',*,*,#2340,.F.);
#3217=ORIENTED_EDGE('',*,*,#2341,.F.);
#3218=ORIENTED_EDGE('',*,*,#2342,.F.);
#3219=ORIENTED_EDGE('',*,*,#2343,.F.);
#3220=ORIENTED_EDGE('',*,*,#2344,.F.);
#3221=ORIENTED_EDGE('',*,*,#2309,.F.);
#3222=ORIENTED_EDGE('',*,*,#2319,.T.);
#3223=ORIENTED_EDGE('',*,*,#2316,.T.);
#3224=ORIENTED_EDGE('',*,*,#2313,.F.);
#3225=ORIENTED_EDGE('',*,*,#2345,.T.);
#3226=ORIENTED_EDGE('',*,*,#2346,.T.);
#3227=ORIENTED_EDGE('',*,*,#2347,.T.);
#3228=ORIENTED_EDGE('',*,*,#2348,.T.);
#3229=ORIENTED_EDGE('',*,*,#2349,.T.);
#3230=ORIENTED_EDGE('',*,*,#2350,.T.);
#3231=ORIENTED_EDGE('',*,*,#2351,.T.);
#3232=ORIENTED_EDGE('',*,*,#2352,.T.);
#3233=ORIENTED_EDGE('',*,*,#2353,.T.);
#3234=ORIENTED_EDGE('',*,*,#2354,.T.);
#3235=ORIENTED_EDGE('',*,*,#2355,.T.);
#3236=ORIENTED_EDGE('',*,*,#2356,.T.);
#3237=ORIENTED_EDGE('',*,*,#2357,.T.);
#3238=ORIENTED_EDGE('',*,*,#2358,.T.);
#3239=ORIENTED_EDGE('',*,*,#2359,.T.);
#3240=ORIENTED_EDGE('',*,*,#2360,.T.);
#3241=ORIENTED_EDGE('',*,*,#2361,.T.);
#3242=ORIENTED_EDGE('',*,*,#2362,.T.);
#3243=ORIENTED_EDGE('',*,*,#2363,.T.);
#3244=ORIENTED_EDGE('',*,*,#2364,.T.);
#3245=ORIENTED_EDGE('',*,*,#2365,.T.);
#3246=ORIENTED_EDGE('',*,*,#2366,.T.);
#3247=ORIENTED_EDGE('',*,*,#2367,.T.);
#3248=ORIENTED_EDGE('',*,*,#2368,.T.);
#3249=ORIENTED_EDGE('',*,*,#2368,.F.);
#3250=ORIENTED_EDGE('',*,*,#2369,.T.);
#3251=ORIENTED_EDGE('',*,*,#2344,.T.);
#3252=ORIENTED_EDGE('',*,*,#2369,.F.);
#3253=ORIENTED_EDGE('',*,*,#2367,.F.);
#3254=ORIENTED_EDGE('',*,*,#2370,.T.);
#3255=ORIENTED_EDGE('',*,*,#2343,.T.);
#3256=ORIENTED_EDGE('',*,*,#2370,.F.);
#3257=ORIENTED_EDGE('',*,*,#2366,.F.);
#3258=ORIENTED_EDGE('',*,*,#2371,.T.);
#3259=ORIENTED_EDGE('',*,*,#2342,.T.);
#3260=ORIENTED_EDGE('',*,*,#2371,.F.);
#3261=ORIENTED_EDGE('',*,*,#2365,.F.);
#3262=ORIENTED_EDGE('',*,*,#2372,.T.);
#3263=ORIENTED_EDGE('',*,*,#2341,.T.);
#3264=ORIENTED_EDGE('',*,*,#2372,.F.);
#3265=ORIENTED_EDGE('',*,*,#2373,.T.);
#3266=ORIENTED_EDGE('',*,*,#2337,.T.);
#3267=ORIENTED_EDGE('',*,*,#2374,.F.);
#3268=ORIENTED_EDGE('',*,*,#2362,.F.);
#3269=ORIENTED_EDGE('',*,*,#2375,.T.);
#3270=ORIENTED_EDGE('',*,*,#2338,.T.);
#3271=ORIENTED_EDGE('',*,*,#2373,.F.);
#3272=ORIENTED_EDGE('',*,*,#2361,.F.);
#3273=ORIENTED_EDGE('',*,*,#2376,.T.);
#3274=ORIENTED_EDGE('',*,*,#2339,.T.);
#3275=ORIENTED_EDGE('',*,*,#2375,.F.);
#3276=ORIENTED_EDGE('',*,*,#2364,.F.);
#3277=ORIENTED_EDGE('',*,*,#2374,.T.);
#3278=ORIENTED_EDGE('',*,*,#2340,.T.);
#3279=ORIENTED_EDGE('',*,*,#2376,.F.);
#3280=ORIENTED_EDGE('',*,*,#2363,.F.);
#3281=ORIENTED_EDGE('',*,*,#2377,.T.);
#3282=ORIENTED_EDGE('',*,*,#2333,.T.);
#3283=ORIENTED_EDGE('',*,*,#2378,.F.);
#3284=ORIENTED_EDGE('',*,*,#2358,.F.);
#3285=ORIENTED_EDGE('',*,*,#2379,.T.);
#3286=ORIENTED_EDGE('',*,*,#2334,.T.);
#3287=ORIENTED_EDGE('',*,*,#2377,.F.);
#3288=ORIENTED_EDGE('',*,*,#2357,.F.);
#3289=ORIENTED_EDGE('',*,*,#2380,.T.);
#3290=ORIENTED_EDGE('',*,*,#2335,.T.);
#3291=ORIENTED_EDGE('',*,*,#2379,.F.);
#3292=ORIENTED_EDGE('',*,*,#2360,.F.);
#3293=ORIENTED_EDGE('',*,*,#2378,.T.);
#3294=ORIENTED_EDGE('',*,*,#2336,.T.);
#3295=ORIENTED_EDGE('',*,*,#2380,.F.);
#3296=ORIENTED_EDGE('',*,*,#2359,.F.);
#3297=ORIENTED_EDGE('',*,*,#2381,.T.);
#3298=ORIENTED_EDGE('',*,*,#2329,.T.);
#3299=ORIENTED_EDGE('',*,*,#2382,.F.);
#3300=ORIENTED_EDGE('',*,*,#2354,.F.);
#3301=ORIENTED_EDGE('',*,*,#2383,.T.);
#3302=ORIENTED_EDGE('',*,*,#2330,.T.);
#3303=ORIENTED_EDGE('',*,*,#2381,.F.);
#3304=ORIENTED_EDGE('',*,*,#2353,.F.);
#3305=ORIENTED_EDGE('',*,*,#2384,.T.);
#3306=ORIENTED_EDGE('',*,*,#2331,.T.);
#3307=ORIENTED_EDGE('',*,*,#2383,.F.);
#3308=ORIENTED_EDGE('',*,*,#2356,.F.);
#3309=ORIENTED_EDGE('',*,*,#2382,.T.);
#3310=ORIENTED_EDGE('',*,*,#2332,.T.);
#3311=ORIENTED_EDGE('',*,*,#2384,.F.);
#3312=ORIENTED_EDGE('',*,*,#2355,.F.);
#3313=ORIENTED_EDGE('',*,*,#2385,.T.);
#3314=ORIENTED_EDGE('',*,*,#2325,.T.);
#3315=ORIENTED_EDGE('',*,*,#2386,.F.);
#3316=ORIENTED_EDGE('',*,*,#2350,.F.);
#3317=ORIENTED_EDGE('',*,*,#2387,.T.);
#3318=ORIENTED_EDGE('',*,*,#2326,.T.);
#3319=ORIENTED_EDGE('',*,*,#2385,.F.);
#3320=ORIENTED_EDGE('',*,*,#2349,.F.);
#3321=ORIENTED_EDGE('',*,*,#2388,.T.);
#3322=ORIENTED_EDGE('',*,*,#2327,.T.);
#3323=ORIENTED_EDGE('',*,*,#2387,.F.);
#3324=ORIENTED_EDGE('',*,*,#2352,.F.);
#3325=ORIENTED_EDGE('',*,*,#2386,.T.);
#3326=ORIENTED_EDGE('',*,*,#2328,.T.);
#3327=ORIENTED_EDGE('',*,*,#2388,.F.);
#3328=ORIENTED_EDGE('',*,*,#2351,.F.);
#3329=ORIENTED_EDGE('',*,*,#2389,.T.);
#3330=ORIENTED_EDGE('',*,*,#2321,.T.);
#3331=ORIENTED_EDGE('',*,*,#2390,.F.);
#3332=ORIENTED_EDGE('',*,*,#2346,.F.);
#3333=ORIENTED_EDGE('',*,*,#2391,.T.);
#3334=ORIENTED_EDGE('',*,*,#2322,.T.);
#3335=ORIENTED_EDGE('',*,*,#2389,.F.);
#3336=ORIENTED_EDGE('',*,*,#2345,.F.);
#3337=ORIENTED_EDGE('',*,*,#2392,.T.);
#3338=ORIENTED_EDGE('',*,*,#2323,.T.);
#3339=ORIENTED_EDGE('',*,*,#2391,.F.);
#3340=ORIENTED_EDGE('',*,*,#2348,.F.);
#3341=ORIENTED_EDGE('',*,*,#2390,.T.);
#3342=ORIENTED_EDGE('',*,*,#2324,.T.);
#3343=ORIENTED_EDGE('',*,*,#2392,.F.);
#3344=ORIENTED_EDGE('',*,*,#2347,.F.);
#3345=ORIENTED_EDGE('',*,*,#2393,.F.);
#3346=ORIENTED_EDGE('',*,*,#2394,.T.);
#3347=ORIENTED_EDGE('',*,*,#2395,.T.);
#3348=ORIENTED_EDGE('',*,*,#2396,.T.);
#3349=ORIENTED_EDGE('',*,*,#2397,.T.);
#3350=ORIENTED_EDGE('',*,*,#2398,.F.);
#3351=ORIENTED_EDGE('',*,*,#2399,.T.);
#3352=ORIENTED_EDGE('',*,*,#2400,.T.);
#3353=ORIENTED_EDGE('',*,*,#2401,.T.);
#3354=ORIENTED_EDGE('',*,*,#2402,.F.);
#3355=ORIENTED_EDGE('',*,*,#2403,.T.);
#3356=ORIENTED_EDGE('',*,*,#2394,.F.);
#3357=ORIENTED_EDGE('',*,*,#2401,.F.);
#3358=ORIENTED_EDGE('',*,*,#2404,.T.);
#3359=ORIENTED_EDGE('',*,*,#2405,.T.);
#3360=ORIENTED_EDGE('',*,*,#2406,.T.);
#3361=ORIENTED_EDGE('',*,*,#2397,.F.);
#3362=ORIENTED_EDGE('',*,*,#2407,.T.);
#3363=ORIENTED_EDGE('',*,*,#2408,.T.);
#3364=ORIENTED_EDGE('',*,*,#2409,.T.);
#3365=ORIENTED_EDGE('',*,*,#2410,.F.);
#3366=ORIENTED_EDGE('',*,*,#2393,.T.);
#3367=ORIENTED_EDGE('',*,*,#2411,.F.);
#3368=ORIENTED_EDGE('',*,*,#2412,.F.);
#3369=ORIENTED_EDGE('',*,*,#2395,.F.);
#3370=ORIENTED_EDGE('',*,*,#2403,.F.);
#3371=ORIENTED_EDGE('',*,*,#2413,.F.);
#3372=ORIENTED_EDGE('',*,*,#2414,.F.);
#3373=ORIENTED_EDGE('',*,*,#2413,.T.);
#3374=ORIENTED_EDGE('',*,*,#2402,.T.);
#3375=ORIENTED_EDGE('',*,*,#2409,.F.);
#3376=ORIENTED_EDGE('',*,*,#2396,.F.);
#3377=ORIENTED_EDGE('',*,*,#2412,.T.);
#3378=ORIENTED_EDGE('',*,*,#2415,.T.);
#3379=ORIENTED_EDGE('',*,*,#2407,.F.);
#3380=ORIENTED_EDGE('',*,*,#2415,.F.);
#3381=ORIENTED_EDGE('',*,*,#2411,.T.);
#3382=ORIENTED_EDGE('',*,*,#2414,.T.);
#3383=ORIENTED_EDGE('',*,*,#2408,.F.);
#3384=ORIENTED_EDGE('',*,*,#2416,.F.);
#3385=ORIENTED_EDGE('',*,*,#2417,.F.);
#3386=ORIENTED_EDGE('',*,*,#2418,.F.);
#3387=ORIENTED_EDGE('',*,*,#2399,.F.);
#3388=ORIENTED_EDGE('',*,*,#2400,.F.);
#3389=ORIENTED_EDGE('',*,*,#2418,.T.);
#3390=ORIENTED_EDGE('',*,*,#2419,.T.);
#3391=ORIENTED_EDGE('',*,*,#2404,.F.);
#3392=ORIENTED_EDGE('',*,*,#2419,.F.);
#3393=ORIENTED_EDGE('',*,*,#2417,.T.);
#3394=ORIENTED_EDGE('',*,*,#2420,.T.);
#3395=ORIENTED_EDGE('',*,*,#2405,.F.);
#3396=ORIENTED_EDGE('',*,*,#2420,.F.);
#3397=ORIENTED_EDGE('',*,*,#2416,.T.);
#3398=ORIENTED_EDGE('',*,*,#2398,.T.);
#3399=ORIENTED_EDGE('',*,*,#2406,.F.);
#3400=ORIENTED_EDGE('',*,*,#2421,.F.);
#3401=ORIENTED_EDGE('',*,*,#2422,.T.);
#3402=ORIENTED_EDGE('',*,*,#2410,.T.);
#3403=ORIENTED_EDGE('',*,*,#2422,.F.);
#3404=ORIENTED_EDGE('',*,*,#2421,.T.);
#3405=ORIENTED_EDGE('',*,*,#2423,.T.);
#3406=ORIENTED_EDGE('',*,*,#2424,.T.);
#3407=ORIENTED_EDGE('',*,*,#2425,.T.);
#3408=ORIENTED_EDGE('',*,*,#2426,.T.);
#3409=ORIENTED_EDGE('',*,*,#2424,.F.);
#3410=ORIENTED_EDGE('',*,*,#2427,.T.);
#3411=ORIENTED_EDGE('',*,*,#2428,.F.);
#3412=ORIENTED_EDGE('',*,*,#2429,.T.);
#3413=ORIENTED_EDGE('',*,*,#2425,.F.);
#3414=ORIENTED_EDGE('',*,*,#2426,.F.);
#3415=ORIENTED_EDGE('',*,*,#2429,.F.);
#3416=ORIENTED_EDGE('',*,*,#2430,.F.);
#3417=ORIENTED_EDGE('',*,*,#2431,.F.);
#3418=ORIENTED_EDGE('',*,*,#2432,.T.);
#3419=ORIENTED_EDGE('',*,*,#2433,.T.);
#3420=ORIENTED_EDGE('',*,*,#2432,.F.);
#3421=ORIENTED_EDGE('',*,*,#2428,.T.);
#3422=ORIENTED_EDGE('',*,*,#2434,.F.);
#3423=ORIENTED_EDGE('',*,*,#2435,.F.);
#3424=ORIENTED_EDGE('',*,*,#2436,.T.);
#3425=ORIENTED_EDGE('',*,*,#2434,.T.);
#3426=ORIENTED_EDGE('',*,*,#2436,.F.);
#3427=ORIENTED_EDGE('',*,*,#2437,.F.);
#3428=ORIENTED_EDGE('',*,*,#2438,.T.);
#3429=ORIENTED_EDGE('',*,*,#2435,.T.);
#3430=ORIENTED_EDGE('',*,*,#2438,.F.);
#3431=ORIENTED_EDGE('',*,*,#2439,.F.);
#3432=ORIENTED_EDGE('',*,*,#2440,.T.);
#3433=ORIENTED_EDGE('',*,*,#2437,.T.);
#3434=ORIENTED_EDGE('',*,*,#2440,.F.);
#3435=ORIENTED_EDGE('',*,*,#2433,.F.);
#3436=ORIENTED_EDGE('',*,*,#2439,.T.);
#3437=ORIENTED_EDGE('',*,*,#2430,.T.);
#3438=ORIENTED_EDGE('',*,*,#2431,.T.);
#3439=ORIENTED_EDGE('',*,*,#2441,.T.);
#3440=ORIENTED_EDGE('',*,*,#2442,.T.);
#3441=ORIENTED_EDGE('',*,*,#2443,.T.);
#3442=ORIENTED_EDGE('',*,*,#2441,.F.);
#3443=ORIENTED_EDGE('',*,*,#2423,.F.);
#3444=ORIENTED_EDGE('',*,*,#2444,.T.);
#3445=ORIENTED_EDGE('',*,*,#2445,.T.);
#3446=ORIENTED_EDGE('',*,*,#2444,.F.);
#3447=ORIENTED_EDGE('',*,*,#2427,.F.);
#3448=ORIENTED_EDGE('',*,*,#2446,.F.);
#3449=ORIENTED_EDGE('',*,*,#2447,.T.);
#3450=ORIENTED_EDGE('',*,*,#2442,.F.);
#3451=ORIENTED_EDGE('',*,*,#2443,.F.);
#3452=ORIENTED_EDGE('',*,*,#2447,.F.);
#3453=ORIENTED_EDGE('',*,*,#2448,.T.);
#3454=ORIENTED_EDGE('',*,*,#2445,.F.);
#3455=ORIENTED_EDGE('',*,*,#2448,.F.);
#3456=ORIENTED_EDGE('',*,*,#2449,.T.);
#3457=ORIENTED_EDGE('',*,*,#2450,.T.);
#3458=ORIENTED_EDGE('',*,*,#2449,.F.);
#3459=ORIENTED_EDGE('',*,*,#2450,.F.);
#3460=ORIENTED_EDGE('',*,*,#2451,.T.);
#3461=ORIENTED_EDGE('',*,*,#2452,.T.);
#3462=ORIENTED_EDGE('',*,*,#2451,.F.);
#3463=ORIENTED_EDGE('',*,*,#2452,.F.);
#3464=ORIENTED_EDGE('',*,*,#2453,.T.);
#3465=ORIENTED_EDGE('',*,*,#2454,.T.);
#3466=ORIENTED_EDGE('',*,*,#2453,.F.);
#3467=ORIENTED_EDGE('',*,*,#2454,.F.);
#3468=ORIENTED_EDGE('',*,*,#2446,.T.);
#3469=ORIENTED_EDGE('',*,*,#2455,.T.);
#3470=ORIENTED_EDGE('',*,*,#2456,.T.);
#3471=ORIENTED_EDGE('',*,*,#2457,.F.);
#3472=ORIENTED_EDGE('',*,*,#2456,.F.);
#3473=ORIENTED_EDGE('',*,*,#2458,.T.);
#3474=ORIENTED_EDGE('',*,*,#2459,.T.);
#3475=ORIENTED_EDGE('',*,*,#2460,.T.);
#3476=ORIENTED_EDGE('',*,*,#2461,.F.);
#3477=ORIENTED_EDGE('',*,*,#2460,.F.);
#3478=ORIENTED_EDGE('',*,*,#2462,.F.);
#3479=ORIENTED_EDGE('',*,*,#2463,.T.);
#3480=ORIENTED_EDGE('',*,*,#2464,.T.);
#3481=ORIENTED_EDGE('',*,*,#2463,.F.);
#3482=ORIENTED_EDGE('',*,*,#2465,.F.);
#3483=ORIENTED_EDGE('',*,*,#2466,.T.);
#3484=ORIENTED_EDGE('',*,*,#2467,.T.);
#3485=ORIENTED_EDGE('',*,*,#2466,.F.);
#3486=ORIENTED_EDGE('',*,*,#2468,.F.);
#3487=ORIENTED_EDGE('',*,*,#2469,.T.);
#3488=ORIENTED_EDGE('',*,*,#2470,.T.);
#3489=ORIENTED_EDGE('',*,*,#2469,.F.);
#3490=ORIENTED_EDGE('',*,*,#2471,.F.);
#3491=ORIENTED_EDGE('',*,*,#2472,.T.);
#3492=ORIENTED_EDGE('',*,*,#2473,.T.);
#3493=ORIENTED_EDGE('',*,*,#2472,.F.);
#3494=ORIENTED_EDGE('',*,*,#2474,.F.);
#3495=ORIENTED_EDGE('',*,*,#2475,.T.);
#3496=ORIENTED_EDGE('',*,*,#2476,.T.);
#3497=ORIENTED_EDGE('',*,*,#2475,.F.);
#3498=ORIENTED_EDGE('',*,*,#2477,.T.);
#3499=ORIENTED_EDGE('',*,*,#2478,.T.);
#3500=ORIENTED_EDGE('',*,*,#2479,.F.);
#3501=ORIENTED_EDGE('',*,*,#2478,.F.);
#3502=ORIENTED_EDGE('',*,*,#2480,.T.);
#3503=ORIENTED_EDGE('',*,*,#2481,.T.);
#3504=ORIENTED_EDGE('',*,*,#2482,.F.);
#3505=ORIENTED_EDGE('',*,*,#2481,.F.);
#3506=ORIENTED_EDGE('',*,*,#2461,.T.);
#3507=ORIENTED_EDGE('',*,*,#2480,.F.);
#3508=ORIENTED_EDGE('',*,*,#2455,.F.);
#3509=ORIENTED_EDGE('',*,*,#2479,.T.);
#3510=ORIENTED_EDGE('',*,*,#2482,.T.);
#3511=ORIENTED_EDGE('',*,*,#2464,.F.);
#3512=ORIENTED_EDGE('',*,*,#2467,.F.);
#3513=ORIENTED_EDGE('',*,*,#2470,.F.);
#3514=ORIENTED_EDGE('',*,*,#2473,.F.);
#3515=ORIENTED_EDGE('',*,*,#2476,.F.);
#3516=ORIENTED_EDGE('',*,*,#2483,.F.);
#3517=ORIENTED_EDGE('',*,*,#2484,.F.);
#3518=ORIENTED_EDGE('',*,*,#2477,.F.);
#3519=ORIENTED_EDGE('',*,*,#2462,.T.);
#3520=ORIENTED_EDGE('',*,*,#2465,.T.);
#3521=ORIENTED_EDGE('',*,*,#2468,.T.);
#3522=ORIENTED_EDGE('',*,*,#2471,.T.);
#3523=ORIENTED_EDGE('',*,*,#2474,.T.);
#3524=ORIENTED_EDGE('',*,*,#2485,.T.);
#3525=ORIENTED_EDGE('',*,*,#2486,.F.);
#3526=ORIENTED_EDGE('',*,*,#2487,.T.);
#3527=ORIENTED_EDGE('',*,*,#2488,.T.);
#3528=ORIENTED_EDGE('',*,*,#2486,.T.);
#3529=ORIENTED_EDGE('',*,*,#2488,.F.);
#3530=ORIENTED_EDGE('',*,*,#2489,.T.);
#3531=ORIENTED_EDGE('',*,*,#2490,.T.);
#3532=ORIENTED_EDGE('',*,*,#2491,.F.);
#3533=ORIENTED_EDGE('',*,*,#2490,.F.);
#3534=ORIENTED_EDGE('',*,*,#2484,.T.);
#3535=ORIENTED_EDGE('',*,*,#2492,.T.);
#3536=ORIENTED_EDGE('',*,*,#2493,.F.);
#3537=ORIENTED_EDGE('',*,*,#2492,.F.);
#3538=ORIENTED_EDGE('',*,*,#2493,.T.);
#3539=ORIENTED_EDGE('',*,*,#2489,.F.);
#3540=ORIENTED_EDGE('',*,*,#2487,.F.);
#3541=ORIENTED_EDGE('',*,*,#2491,.T.);
#3542=ORIENTED_EDGE('',*,*,#2485,.F.);
#3543=ORIENTED_EDGE('',*,*,#2494,.T.);
#3544=ORIENTED_EDGE('',*,*,#2483,.T.);
#3545=ORIENTED_EDGE('',*,*,#2494,.F.);
#3546=ORIENTED_EDGE('',*,*,#2457,.T.);
#3547=ORIENTED_EDGE('',*,*,#2495,.T.);
#3548=ORIENTED_EDGE('',*,*,#2496,.F.);
#3549=ORIENTED_EDGE('',*,*,#2497,.F.);
#3550=ORIENTED_EDGE('',*,*,#2495,.F.);
#3551=ORIENTED_EDGE('',*,*,#2458,.F.);
#3552=ORIENTED_EDGE('',*,*,#2459,.F.);
#3553=ORIENTED_EDGE('',*,*,#2498,.T.);
#3554=ORIENTED_EDGE('',*,*,#2499,.T.);
#3555=ORIENTED_EDGE('',*,*,#2498,.F.);
#3556=ORIENTED_EDGE('',*,*,#2499,.F.);
#3557=ORIENTED_EDGE('',*,*,#2500,.T.);
#3558=ORIENTED_EDGE('',*,*,#2496,.T.);
#3559=ORIENTED_EDGE('',*,*,#2497,.T.);
#3560=ORIENTED_EDGE('',*,*,#2500,.F.);
#3561=ORIENTED_EDGE('',*,*,#2501,.F.);
#3562=ORIENTED_EDGE('',*,*,#2502,.T.);
#3563=ORIENTED_EDGE('',*,*,#2503,.T.);
#3564=ORIENTED_EDGE('',*,*,#2504,.F.);
#3565=ORIENTED_EDGE('',*,*,#2505,.F.);
#3566=ORIENTED_EDGE('',*,*,#2506,.T.);
#3567=ORIENTED_EDGE('',*,*,#2501,.T.);
#3568=ORIENTED_EDGE('',*,*,#2507,.F.);
#3569=ORIENTED_EDGE('',*,*,#2508,.F.);
#3570=ORIENTED_EDGE('',*,*,#2509,.T.);
#3571=ORIENTED_EDGE('',*,*,#2505,.T.);
#3572=ORIENTED_EDGE('',*,*,#2510,.F.);
#3573=ORIENTED_EDGE('',*,*,#2502,.F.);
#3574=ORIENTED_EDGE('',*,*,#2511,.F.);
#3575=ORIENTED_EDGE('',*,*,#2512,.T.);
#3576=ORIENTED_EDGE('',*,*,#2513,.T.);
#3577=ORIENTED_EDGE('',*,*,#2511,.T.);
#3578=ORIENTED_EDGE('',*,*,#2506,.F.);
#3579=ORIENTED_EDGE('',*,*,#2514,.F.);
#3580=ORIENTED_EDGE('',*,*,#2515,.T.);
#3581=ORIENTED_EDGE('',*,*,#2514,.T.);
#3582=ORIENTED_EDGE('',*,*,#2509,.F.);
#3583=ORIENTED_EDGE('',*,*,#2516,.F.);
#3584=ORIENTED_EDGE('',*,*,#2517,.T.);
#3585=ORIENTED_EDGE('',*,*,#2516,.T.);
#3586=ORIENTED_EDGE('',*,*,#2518,.F.);
#3587=ORIENTED_EDGE('',*,*,#2513,.F.);
#3588=ORIENTED_EDGE('',*,*,#2519,.T.);
#3589=ORIENTED_EDGE('',*,*,#2512,.F.);
#3590=ORIENTED_EDGE('',*,*,#2520,.F.);
#3591=ORIENTED_EDGE('',*,*,#2521,.T.);
#3592=ORIENTED_EDGE('',*,*,#2522,.T.);
#3593=ORIENTED_EDGE('',*,*,#2520,.T.);
#3594=ORIENTED_EDGE('',*,*,#2515,.F.);
#3595=ORIENTED_EDGE('',*,*,#2523,.F.);
#3596=ORIENTED_EDGE('',*,*,#2524,.T.);
#3597=ORIENTED_EDGE('',*,*,#2523,.T.);
#3598=ORIENTED_EDGE('',*,*,#2517,.F.);
#3599=ORIENTED_EDGE('',*,*,#2525,.F.);
#3600=ORIENTED_EDGE('',*,*,#2526,.T.);
#3601=ORIENTED_EDGE('',*,*,#2525,.T.);
#3602=ORIENTED_EDGE('',*,*,#2519,.F.);
#3603=ORIENTED_EDGE('',*,*,#2522,.F.);
#3604=ORIENTED_EDGE('',*,*,#2527,.T.);
#3605=ORIENTED_EDGE('',*,*,#2521,.F.);
#3606=ORIENTED_EDGE('',*,*,#2528,.F.);
#3607=ORIENTED_EDGE('',*,*,#2504,.T.);
#3608=ORIENTED_EDGE('',*,*,#2529,.T.);
#3609=ORIENTED_EDGE('',*,*,#2528,.T.);
#3610=ORIENTED_EDGE('',*,*,#2524,.F.);
#3611=ORIENTED_EDGE('',*,*,#2530,.F.);
#3612=ORIENTED_EDGE('',*,*,#2507,.T.);
#3613=ORIENTED_EDGE('',*,*,#2530,.T.);
#3614=ORIENTED_EDGE('',*,*,#2526,.F.);
#3615=ORIENTED_EDGE('',*,*,#2531,.F.);
#3616=ORIENTED_EDGE('',*,*,#2510,.T.);
#3617=ORIENTED_EDGE('',*,*,#2531,.T.);
#3618=ORIENTED_EDGE('',*,*,#2527,.F.);
#3619=ORIENTED_EDGE('',*,*,#2529,.F.);
#3620=ORIENTED_EDGE('',*,*,#2532,.T.);
#3621=ORIENTED_EDGE('',*,*,#2518,.T.);
#3622=ORIENTED_EDGE('',*,*,#2508,.T.);
#3623=ORIENTED_EDGE('',*,*,#2532,.F.);
#3624=ORIENTED_EDGE('',*,*,#2503,.F.);
#3625=PLANE('',#4037);
#3626=PLANE('',#4042);
#3627=PLANE('',#4043);
#3628=PLANE('',#4044);
#3629=PLANE('',#4045);
#3630=PLANE('',#4046);
#3631=PLANE('',#4047);
#3632=PLANE('',#4052);
#3633=PLANE('',#4053);
#3634=PLANE('',#4054);
#3635=PLANE('',#4055);
#3636=PLANE('',#4056);
#3637=PLANE('',#4059);
#3638=PLANE('',#4060);
#3639=PLANE('',#4061);
#3640=PLANE('',#4062);
#3641=PLANE('',#4065);
#3642=PLANE('',#4066);
#3643=PLANE('',#4068);
#3644=PLANE('',#4070);
#3645=PLANE('',#4072);
#3646=PLANE('',#4074);
#3647=PLANE('',#4075);
#3648=PLANE('',#4076);
#3649=PLANE('',#4078);
#3650=PLANE('',#4080);
#3651=PLANE('',#4081);
#3652=PLANE('',#4083);
#3653=PLANE('',#4085);
#3654=PLANE('',#4086);
#3655=PLANE('',#4087);
#3656=PLANE('',#4088);
#3657=PLANE('',#4089);
#3658=PLANE('',#4090);
#3659=PLANE('',#4091);
#3660=PLANE('',#4092);
#3661=PLANE('',#4097);
#3662=PLANE('',#4099);
#3663=PLANE('',#4102);
#3664=PLANE('',#4104);
#3665=PLANE('',#4106);
#3666=PLANE('',#4109);
#3667=PLANE('',#4111);
#3668=PLANE('',#4112);
#3669=PLANE('',#4113);
#3670=PLANE('',#4114);
#3671=PLANE('',#4115);
#3672=PLANE('',#4116);
#3673=PLANE('',#4117);
#3674=PLANE('',#4118);
#3675=PLANE('',#4119);
#3676=PLANE('',#4120);
#3677=PLANE('',#4121);
#3678=PLANE('',#4122);
#3679=PLANE('',#4123);
#3680=PLANE('',#4124);
#3681=PLANE('',#4125);
#3682=PLANE('',#4126);
#3683=PLANE('',#4127);
#3684=PLANE('',#4128);
#3685=PLANE('',#4129);
#3686=PLANE('',#4130);
#3687=PLANE('',#4131);
#3688=PLANE('',#4132);
#3689=PLANE('',#4133);
#3690=PLANE('',#4134);
#3691=PLANE('',#4135);
#3692=PLANE('',#4136);
#3693=PLANE('',#4137);
#3694=PLANE('',#4138);
#3695=PLANE('',#4139);
#3696=PLANE('',#4140);
#3697=PLANE('',#4141);
#3698=PLANE('',#4142);
#3699=PLANE('',#4226);
#3700=PLANE('',#4227);
#3701=PLANE('',#4228);
#3702=PLANE('',#4229);
#3703=PLANE('',#4230);
#3704=PLANE('',#4245);
#3705=PLANE('',#4265);
#3706=PLANE('',#4267);
#3707=PLANE('',#4269);
#3708=PLANE('',#4271);
#3709=PLANE('',#4273);
#3710=PLANE('',#4275);
#3711=PLANE('',#4277);
#3712=PLANE('',#4279);
#3713=PLANE('',#4281);
#3714=PLANE('',#4283);
#3715=PLANE('',#4295);
#3716=PLANE('',#4297);
#3717=PLANE('',#4298);
#3718=PLANE('',#4299);
#3719=PLANE('',#4300);
#3720=PLANE('',#4301);
#3721=PLANE('',#4302);
#3722=PLANE('',#4303);
#3723=PLANE('',#4304);
#3724=PLANE('',#4305);
#3725=PLANE('',#4308);
#3726=PLANE('',#4322);
#3727=PLANE('',#4332);
#3728=PLANE('',#4341);
#3729=PLANE('',#4351);
#3730=PLANE('',#4381);
#3731=PLANE('',#4382);
#3732=PLANE('',#4383);
#3733=PLANE('',#4386);
#3734=PLANE('',#4396);
#3735=PLANE('',#4397);
#3736=PLANE('',#4406);
#3737=PLANE('',#4407);
#3738=PLANE('',#4408);
#3739=PLANE('',#4415);
#3740=PLANE('',#4416);
#3741=PLANE('',#4417);
#3742=PLANE('',#4418);
#3743=PLANE('',#4425);
#3744=ADVANCED_FACE('',(#394,#185,#186,#187,#188,#189,#190),#3625,.T.);
#3745=ADVANCED_FACE('',(#395),#3626,.F.);
#3746=ADVANCED_FACE('',(#396),#3627,.F.);
#3747=ADVANCED_FACE('',(#397),#3628,.T.);
#3748=ADVANCED_FACE('',(#398),#3629,.T.);
#3749=ADVANCED_FACE('',(#399),#3630,.T.);
#3750=ADVANCED_FACE('',(#400,#191,#192,#193,#194,#195,#196),#3631,.F.);
#3751=ADVANCED_FACE('',(#401),#3632,.T.);
#3752=ADVANCED_FACE('',(#402),#3633,.T.);
#3753=ADVANCED_FACE('',(#403),#3634,.T.);
#3754=ADVANCED_FACE('',(#404),#3635,.T.);
#3755=ADVANCED_FACE('',(#405,#197,#198),#3636,.F.);
#3756=ADVANCED_FACE('',(#406),#3637,.T.);
#3757=ADVANCED_FACE('',(#407),#3638,.T.);
#3758=ADVANCED_FACE('',(#408),#3639,.F.);
#3759=ADVANCED_FACE('',(#409,#199,#200),#3640,.T.);
#3760=ADVANCED_FACE('',(#410),#3641,.F.);
#3761=ADVANCED_FACE('',(#411),#3642,.F.);
#3762=ADVANCED_FACE('',(#412),#3643,.F.);
#3763=ADVANCED_FACE('',(#413),#3644,.F.);
#3764=ADVANCED_FACE('',(#414),#3645,.F.);
#3765=ADVANCED_FACE('',(#415),#3646,.F.);
#3766=ADVANCED_FACE('',(#416),#3647,.F.);
#3767=ADVANCED_FACE('',(#417),#3648,.F.);
#3768=ADVANCED_FACE('',(#418),#3649,.F.);
#3769=ADVANCED_FACE('',(#419),#3650,.F.);
#3770=ADVANCED_FACE('',(#420),#3651,.F.);
#3771=ADVANCED_FACE('',(#421),#3652,.F.);
#3772=ADVANCED_FACE('',(#422),#3653,.T.);
#3773=ADVANCED_FACE('',(#423),#3654,.T.);
#3774=ADVANCED_FACE('',(#424),#3655,.F.);
#3775=ADVANCED_FACE('',(#425),#3656,.F.);
#3776=ADVANCED_FACE('',(#426),#3657,.T.);
#3777=ADVANCED_FACE('',(#427),#3658,.T.);
#3778=ADVANCED_FACE('',(#428),#3659,.F.);
#3779=ADVANCED_FACE('',(#429),#3660,.F.);
#3780=ADVANCED_FACE('',(#430),#108,.F.);
#3781=ADVANCED_FACE('',(#431),#109,.F.);
#3782=ADVANCED_FACE('',(#432),#110,.F.);
#3783=ADVANCED_FACE('',(#433),#111,.F.);
#3784=ADVANCED_FACE('',(#434),#3661,.F.);
#3785=ADVANCED_FACE('',(#435),#3662,.F.);
#3786=ADVANCED_FACE('',(#436),#3663,.F.);
#3787=ADVANCED_FACE('',(#437),#3664,.F.);
#3788=ADVANCED_FACE('',(#438),#3665,.F.);
#3789=ADVANCED_FACE('',(#439),#3666,.F.);
#3790=ADVANCED_FACE('',(#440),#3667,.T.);
#3791=ADVANCED_FACE('',(#441),#3668,.T.);
#3792=ADVANCED_FACE('',(#442),#3669,.T.);
#3793=ADVANCED_FACE('',(#443),#3670,.T.);
#3794=ADVANCED_FACE('',(#444),#3671,.F.);
#3795=ADVANCED_FACE('',(#445),#3672,.T.);
#3796=ADVANCED_FACE('',(#446),#3673,.T.);
#3797=ADVANCED_FACE('',(#447),#3674,.T.);
#3798=ADVANCED_FACE('',(#448),#3675,.T.);
#3799=ADVANCED_FACE('',(#449),#3676,.T.);
#3800=ADVANCED_FACE('',(#450),#3677,.T.);
#3801=ADVANCED_FACE('',(#451),#3678,.F.);
#3802=ADVANCED_FACE('',(#452),#3679,.T.);
#3803=ADVANCED_FACE('',(#453),#3680,.T.);
#3804=ADVANCED_FACE('',(#454),#3681,.T.);
#3805=ADVANCED_FACE('',(#455),#3682,.T.);
#3806=ADVANCED_FACE('',(#456),#3683,.F.);
#3807=ADVANCED_FACE('',(#457),#3684,.T.);
#3808=ADVANCED_FACE('',(#458),#3685,.T.);
#3809=ADVANCED_FACE('',(#459),#3686,.T.);
#3810=ADVANCED_FACE('',(#460),#3687,.T.);
#3811=ADVANCED_FACE('',(#461),#3688,.T.);
#3812=ADVANCED_FACE('',(#462),#3689,.T.);
#3813=ADVANCED_FACE('',(#463),#3690,.F.);
#3814=ADVANCED_FACE('',(#464),#3691,.T.);
#3815=ADVANCED_FACE('',(#465),#3692,.T.);
#3816=ADVANCED_FACE('',(#466),#3693,.F.);
#3817=ADVANCED_FACE('',(#467),#3694,.T.);
#3818=ADVANCED_FACE('',(#468),#3695,.T.);
#3819=ADVANCED_FACE('',(#469),#3696,.T.);
#3820=ADVANCED_FACE('',(#470),#3697,.T.);
#3821=ADVANCED_FACE('',(#471),#3698,.F.);
#3822=ADVANCED_FACE('',(#472),#112,.T.);
#3823=ADVANCED_FACE('',(#473),#113,.T.);
#3824=ADVANCED_FACE('',(#474),#114,.T.);
#3825=ADVANCED_FACE('',(#475),#78,.T.);
#3826=ADVANCED_FACE('',(#476),#115,.T.);
#3827=ADVANCED_FACE('',(#477),#116,.F.);
#3828=ADVANCED_FACE('',(#478),#117,.T.);
#3829=ADVANCED_FACE('',(#479),#118,.F.);
#3830=ADVANCED_FACE('',(#480),#79,.T.);
#3831=ADVANCED_FACE('',(#481),#119,.T.);
#3832=ADVANCED_FACE('',(#482),#120,.T.);
#3833=ADVANCED_FACE('',(#483),#121,.T.);
#3834=ADVANCED_FACE('',(#484),#122,.T.);
#3835=ADVANCED_FACE('',(#485),#80,.T.);
#3836=ADVANCED_FACE('',(#486),#123,.T.);
#3837=ADVANCED_FACE('',(#487),#124,.F.);
#3838=ADVANCED_FACE('',(#488),#125,.T.);
#3839=ADVANCED_FACE('',(#489),#126,.F.);
#3840=ADVANCED_FACE('',(#490),#81,.T.);
#3841=ADVANCED_FACE('',(#491),#127,.T.);
#3842=ADVANCED_FACE('',(#492),#128,.T.);
#3843=ADVANCED_FACE('',(#493),#129,.T.);
#3844=ADVANCED_FACE('',(#494),#130,.T.);
#3845=ADVANCED_FACE('',(#495),#82,.T.);
#3846=ADVANCED_FACE('',(#496),#131,.T.);
#3847=ADVANCED_FACE('',(#497),#132,.F.);
#3848=ADVANCED_FACE('',(#498),#133,.T.);
#3849=ADVANCED_FACE('',(#499),#134,.F.);
#3850=ADVANCED_FACE('',(#500),#83,.T.);
#3851=ADVANCED_FACE('',(#501),#135,.T.);
#3852=ADVANCED_FACE('',(#502),#136,.T.);
#3853=ADVANCED_FACE('',(#503),#137,.T.);
#3854=ADVANCED_FACE('',(#504),#84,.T.);
#3855=ADVANCED_FACE('',(#505),#138,.T.);
#3856=ADVANCED_FACE('',(#506),#139,.F.);
#3857=ADVANCED_FACE('',(#507),#140,.T.);
#3858=ADVANCED_FACE('',(#508),#141,.F.);
#3859=ADVANCED_FACE('',(#509),#142,.T.);
#3860=ADVANCED_FACE('',(#510),#85,.T.);
#3861=ADVANCED_FACE('',(#511),#143,.T.);
#3862=ADVANCED_FACE('',(#512),#144,.F.);
#3863=ADVANCED_FACE('',(#513),#145,.F.);
#3864=ADVANCED_FACE('',(#514),#3699,.F.);
#3865=ADVANCED_FACE('',(#515),#3700,.F.);
#3866=ADVANCED_FACE('',(#516),#3701,.T.);
#3867=ADVANCED_FACE('',(#517),#3702,.T.);
#3868=ADVANCED_FACE('',(#518,#201,#202,#203,#204,#205,#206,#207,#208,#209),
#3703,.T.);
#3869=ADVANCED_FACE('',(#519,#210,#211,#212,#213,#214,#215,#216,#217,#218),
#3704,.F.);
#3870=ADVANCED_FACE('',(#520),#146,.F.);
#3871=ADVANCED_FACE('',(#521),#147,.F.);
#3872=ADVANCED_FACE('',(#522),#148,.F.);
#3873=ADVANCED_FACE('',(#523),#149,.F.);
#3874=ADVANCED_FACE('',(#524),#150,.F.);
#3875=ADVANCED_FACE('',(#525),#3705,.F.);
#3876=ADVANCED_FACE('',(#526),#151,.F.);
#3877=ADVANCED_FACE('',(#527),#3706,.F.);
#3878=ADVANCED_FACE('',(#528),#152,.F.);
#3879=ADVANCED_FACE('',(#529),#3707,.F.);
#3880=ADVANCED_FACE('',(#530),#153,.F.);
#3881=ADVANCED_FACE('',(#531),#3708,.F.);
#3882=ADVANCED_FACE('',(#532),#154,.F.);
#3883=ADVANCED_FACE('',(#533),#3709,.F.);
#3884=ADVANCED_FACE('',(#534),#155,.F.);
#3885=ADVANCED_FACE('',(#535),#3710,.F.);
#3886=ADVANCED_FACE('',(#536),#156,.F.);
#3887=ADVANCED_FACE('',(#537),#3711,.F.);
#3888=ADVANCED_FACE('',(#538),#157,.F.);
#3889=ADVANCED_FACE('',(#539),#3712,.F.);
#3890=ADVANCED_FACE('',(#540),#158,.F.);
#3891=ADVANCED_FACE('',(#541),#3713,.F.);
#3892=ADVANCED_FACE('',(#542),#159,.F.);
#3893=ADVANCED_FACE('',(#543),#3714,.F.);
#3894=ADVANCED_FACE('',(#544),#160,.T.);
#3895=ADVANCED_FACE('',(#545,#219),#3715,.F.);
#3896=ADVANCED_FACE('',(#546),#3716,.T.);
#3897=ADVANCED_FACE('',(#547),#3717,.T.);
#3898=ADVANCED_FACE('',(#548),#3718,.T.);
#3899=ADVANCED_FACE('',(#549),#3719,.T.);
#3900=ADVANCED_FACE('',(#550),#3720,.T.);
#3901=ADVANCED_FACE('',(#551),#3721,.T.);
#3902=ADVANCED_FACE('',(#552),#3722,.T.);
#3903=ADVANCED_FACE('',(#553),#3723,.T.);
#3904=ADVANCED_FACE('',(#554),#3724,.T.);
#3905=ADVANCED_FACE('',(#555),#15,.F.);
#3906=ADVANCED_FACE('',(#556),#3725,.T.);
#3907=ADVANCED_FACE('',(#557),#86,.T.);
#3908=ADVANCED_FACE('',(#558),#161,.T.);
#3909=ADVANCED_FACE('',(#559),#162,.T.);
#3910=ADVANCED_FACE('',(#560,#220),#3726,.T.);
#3911=ADVANCED_FACE('',(#561),#87,.T.);
#3912=ADVANCED_FACE('',(#562),#163,.F.);
#3913=ADVANCED_FACE('',(#563),#88,.T.);
#3914=ADVANCED_FACE('',(#564,#221),#3727,.T.);
#3915=ADVANCED_FACE('',(#565),#89,.T.);
#3916=ADVANCED_FACE('',(#566),#164,.F.);
#3917=ADVANCED_FACE('',(#567),#165,.F.);
#3918=ADVANCED_FACE('',(#568,#222),#3728,.T.);
#3919=ADVANCED_FACE('',(#569),#90,.T.);
#3920=ADVANCED_FACE('',(#570),#166,.T.);
#3921=ADVANCED_FACE('',(#571),#91,.T.);
#3922=ADVANCED_FACE('',(#572,#223),#3729,.T.);
#3923=ADVANCED_FACE('',(#573),#167,.T.);
#3924=ADVANCED_FACE('',(#574),#168,.T.);
#3925=ADVANCED_FACE('',(#575),#169,.F.);
#3926=ADVANCED_FACE('',(#576),#170,.F.);
#3927=ADVANCED_FACE('',(#577),#171,.F.);
#3928=ADVANCED_FACE('',(#578),#172,.F.);
#3929=ADVANCED_FACE('',(#579),#173,.F.);
#3930=ADVANCED_FACE('',(#580),#174,.F.);
#3931=ADVANCED_FACE('',(#581),#175,.F.);
#3932=ADVANCED_FACE('',(#582,#224),#3730,.T.);
#3933=ADVANCED_FACE('',(#583,#225),#3731,.F.);
#3934=ADVANCED_FACE('',(#584,#226,#227,#228,#229,#230,#231,#232),#3732,
 .T.);
#3935=ADVANCED_FACE('',(#585,#233,#234,#235,#236,#237,#238,#239),#3733,
 .F.);
#3936=ADVANCED_FACE('',(#586),#176,.T.);
#3937=ADVANCED_FACE('',(#587),#177,.F.);
#3938=ADVANCED_FACE('',(#588),#178,.T.);
#3939=ADVANCED_FACE('',(#589,#240),#3734,.T.);
#3940=ADVANCED_FACE('',(#590,#241),#3735,.F.);
#3941=ADVANCED_FACE('',(#591),#179,.F.);
#3942=ADVANCED_FACE('',(#592),#16,.T.);
#3943=ADVANCED_FACE('',(#593),#17,.T.);
#3944=ADVANCED_FACE('',(#594),#180,.T.);
#3945=ADVANCED_FACE('',(#595),#3736,.T.);
#3946=ADVANCED_FACE('',(#596),#3737,.T.);
#3947=ADVANCED_FACE('',(#597),#3738,.T.);
#3948=ADVANCED_FACE('',(#598),#181,.T.);
#3949=ADVANCED_FACE('',(#599),#11,.T.);
#3950=ADVANCED_FACE('',(#600),#182,.F.);
#3951=ADVANCED_FACE('',(#601),#12,.T.);
#3952=ADVANCED_FACE('',(#602),#3739,.T.);
#3953=ADVANCED_FACE('',(#603),#3740,.T.);
#3954=ADVANCED_FACE('',(#604),#3741,.T.);
#3955=ADVANCED_FACE('',(#605),#3742,.T.);
#3956=ADVANCED_FACE('',(#606),#183,.T.);
#3957=ADVANCED_FACE('',(#607),#13,.T.);
#3958=ADVANCED_FACE('',(#608),#184,.F.);
#3959=ADVANCED_FACE('',(#609),#14,.T.);
#3960=ADVANCED_FACE('',(#610),#3743,.T.);
#3961=CLOSED_SHELL('',(#3744,#3745,#3746,#3747,#3748,#3749,#3750,#3751,
#3752,#3753,#3754,#3755,#3756,#3757,#3758,#3759,#3760,#3761,#3762,#3763,
#3764,#3765,#3766,#3767,#3768,#3769,#3770,#3771,#3772,#3773,#3774,#3775,
#3776,#3777,#3778,#3779,#3780,#3781,#3782,#3783,#3784,#3785,#3786,#3787,
#3788,#3789,#3790,#3791,#3792,#3793,#3794,#3795,#3796,#3797,#3798,#3799,
#3800,#3801,#3802,#3803,#3804,#3805,#3806,#3807,#3808,#3809,#3810,#3811,
#3812,#3813,#3814,#3815,#3816,#3817,#3818,#3819,#3820,#3821,#3822,#3823,
#3824,#3825,#3826,#3827,#3828,#3829,#3830,#3831,#3832,#3833,#3834,#3835,
#3836,#3837,#3838,#3839,#3840,#3841,#3842,#3843,#3844,#3845,#3846,#3847,
#3848,#3849,#3850,#3851,#3852,#3853,#3854,#3855,#3856,#3857,#3858,#3859,
#3860,#3861,#3862,#3863));
#3962=CLOSED_SHELL('',(#3864,#3865,#3866,#3867,#3868,#3869,#3870,#3871,
#3872,#3873,#3874,#3875,#3876,#3877,#3878,#3879,#3880,#3881,#3882,#3883,
#3884,#3885,#3886,#3887,#3888,#3889,#3890,#3891,#3892,#3893));
#3963=CLOSED_SHELL('',(#3894,#3895,#3896,#3897,#3898,#3899,#3900,#3901,
#3902,#3903,#3904,#3905,#3906));
#3964=CLOSED_SHELL('',(#3907,#3908,#3909,#3910,#3911,#3912,#3913,#3914,
#3915,#3916,#3917,#3918,#3919,#3920,#3921,#3922));
#3965=CLOSED_SHELL('',(#3923,#3924,#3925,#3926,#3927,#3928,#3929,#3930,
#3931,#3932,#3933,#3934,#3935,#3936,#3937,#3938,#3939,#3940,#3941,#3942,
#3943,#3944));
#3966=CLOSED_SHELL('',(#3945,#3946,#3947,#3948,#3949,#3950,#3951,#3952,
#3953,#3954,#3955,#3956,#3957,#3958,#3959,#3960));
#3967=DERIVED_UNIT_ELEMENT(#3979,1.);
#3968=DERIVED_UNIT_ELEMENT(#6791,-3.);
#3969=DERIVED_UNIT_ELEMENT(#3979,1.);
#3970=DERIVED_UNIT_ELEMENT(#6791,-3.);
#3971=DERIVED_UNIT_ELEMENT(#3979,1.);
#3972=DERIVED_UNIT_ELEMENT(#6791,-3.);
#3973=DERIVED_UNIT_ELEMENT(#3979,1.);
#3974=DERIVED_UNIT_ELEMENT(#6791,-3.);
#3975=DERIVED_UNIT_ELEMENT(#3979,1.);
#3976=DERIVED_UNIT_ELEMENT(#6791,-3.);
#3977=DERIVED_UNIT_ELEMENT(#3979,1.);
#3978=DERIVED_UNIT_ELEMENT(#6791,-3.);
#3979=(
MASS_UNIT()
NAMED_UNIT(*)
SI_UNIT(.KILO.,.GRAM.)
);
#3980=DERIVED_UNIT((#3967,#3968));
#3981=DERIVED_UNIT((#3969,#3970));
#3982=DERIVED_UNIT((#3971,#3972));
#3983=DERIVED_UNIT((#3973,#3974));
#3984=DERIVED_UNIT((#3975,#3976));
#3985=DERIVED_UNIT((#3977,#3978));
#3986=MEASURE_REPRESENTATION_ITEM('density measure',
POSITIVE_RATIO_MEASURE(7850.),#3980);
#3987=MEASURE_REPRESENTATION_ITEM('density measure',
POSITIVE_RATIO_MEASURE(7850.),#3981);
#3988=MEASURE_REPRESENTATION_ITEM('density measure',
POSITIVE_RATIO_MEASURE(7850.),#3982);
#3989=MEASURE_REPRESENTATION_ITEM('density measure',
POSITIVE_RATIO_MEASURE(7850.),#3983);
#3990=MEASURE_REPRESENTATION_ITEM('density measure',
POSITIVE_RATIO_MEASURE(7850.),#3984);
#3991=MEASURE_REPRESENTATION_ITEM('density measure',
POSITIVE_RATIO_MEASURE(7850.),#3985);
#3992=PROPERTY_DEFINITION_REPRESENTATION(#4022,#4004);
#3993=PROPERTY_DEFINITION_REPRESENTATION(#4023,#4005);
#3994=PROPERTY_DEFINITION_REPRESENTATION(#4024,#4006);
#3995=PROPERTY_DEFINITION_REPRESENTATION(#4025,#4007);
#3996=PROPERTY_DEFINITION_REPRESENTATION(#4026,#4008);
#3997=PROPERTY_DEFINITION_REPRESENTATION(#4027,#4009);
#3998=PROPERTY_DEFINITION_REPRESENTATION(#4028,#4010);
#3999=PROPERTY_DEFINITION_REPRESENTATION(#4029,#4011);
#4000=PROPERTY_DEFINITION_REPRESENTATION(#4030,#4012);
#4001=PROPERTY_DEFINITION_REPRESENTATION(#4031,#4013);
#4002=PROPERTY_DEFINITION_REPRESENTATION(#4032,#4014);
#4003=PROPERTY_DEFINITION_REPRESENTATION(#4033,#4015);
#4004=REPRESENTATION('material name',(#4016),#6783);
#4005=REPRESENTATION('density',(#3986),#6783);
#4006=REPRESENTATION('material name',(#4017),#6784);
#4007=REPRESENTATION('density',(#3987),#6784);
#4008=REPRESENTATION('material name',(#4018),#6785);
#4009=REPRESENTATION('density',(#3988),#6785);
#4010=REPRESENTATION('material name',(#4019),#6786);
#4011=REPRESENTATION('density',(#3989),#6786);
#4012=REPRESENTATION('material name',(#4020),#6787);
#4013=REPRESENTATION('density',(#3990),#6787);
#4014=REPRESENTATION('material name',(#4021),#6788);
#4015=REPRESENTATION('density',(#3991),#6788);
#4016=DESCRIPTIVE_REPRESENTATION_ITEM('Steel','Steel');
#4017=DESCRIPTIVE_REPRESENTATION_ITEM('Steel','Steel');
#4018=DESCRIPTIVE_REPRESENTATION_ITEM('Steel','Steel');
#4019=DESCRIPTIVE_REPRESENTATION_ITEM('Steel','Steel');
#4020=DESCRIPTIVE_REPRESENTATION_ITEM('Steel','Steel');
#4021=DESCRIPTIVE_REPRESENTATION_ITEM('Steel','Steel');
#4022=PROPERTY_DEFINITION('material property','material name',#6830);
#4023=PROPERTY_DEFINITION('material property','density of part',#6830);
#4024=PROPERTY_DEFINITION('material property','material name',#6831);
#4025=PROPERTY_DEFINITION('material property','density of part',#6831);
#4026=PROPERTY_DEFINITION('material property','material name',#6832);
#4027=PROPERTY_DEFINITION('material property','density of part',#6832);
#4028=PROPERTY_DEFINITION('material property','material name',#6833);
#4029=PROPERTY_DEFINITION('material property','density of part',#6833);
#4030=PROPERTY_DEFINITION('material property','material name',#6834);
#4031=PROPERTY_DEFINITION('material property','density of part',#6834);
#4032=PROPERTY_DEFINITION('material property','material name',#6835);
#4033=PROPERTY_DEFINITION('material property','density of part',#6835);
#4034=AXIS2_PLACEMENT_3D('',#5606,#4432,#4433);
#4035=AXIS2_PLACEMENT_3D('',#5607,#4434,#4435);
#4036=AXIS2_PLACEMENT_3D('',#5608,#4436,#4437);
#4037=AXIS2_PLACEMENT_3D('',#5609,#4438,#4439);
#4038=AXIS2_PLACEMENT_3D('',#5635,#4452,#4453);
#4039=AXIS2_PLACEMENT_3D('',#5637,#4454,#4455);
#4040=AXIS2_PLACEMENT_3D('',#5639,#4456,#4457);
#4041=AXIS2_PLACEMENT_3D('',#5641,#4458,#4459);
#4042=AXIS2_PLACEMENT_3D('',#5658,#4468,#4469);
#4043=AXIS2_PLACEMENT_3D('',#5672,#4477,#4478);
#4044=AXIS2_PLACEMENT_3D('',#5694,#4490,#4491);
#4045=AXIS2_PLACEMENT_3D('',#5705,#4498,#4499);
#4046=AXIS2_PLACEMENT_3D('',#5718,#4506,#4507);
#4047=AXIS2_PLACEMENT_3D('',#5731,#4514,#4515);
#4048=AXIS2_PLACEMENT_3D('',#5765,#4532,#4533);
#4049=AXIS2_PLACEMENT_3D('',#5767,#4534,#4535);
#4050=AXIS2_PLACEMENT_3D('',#5769,#4536,#4537);
#4051=AXIS2_PLACEMENT_3D('',#5771,#4538,#4539);
#4052=AXIS2_PLACEMENT_3D('',#5780,#4544,#4545);
#4053=AXIS2_PLACEMENT_3D('',#5789,#4550,#4551);
#4054=AXIS2_PLACEMENT_3D('',#5795,#4555,#4556);
#4055=AXIS2_PLACEMENT_3D('',#5805,#4562,#4563);
#4056=AXIS2_PLACEMENT_3D('',#5815,#4569,#4570);
#4057=AXIS2_PLACEMENT_3D('',#5817,#4571,#4572);
#4058=AXIS2_PLACEMENT_3D('',#5819,#4573,#4574);
#4059=AXIS2_PLACEMENT_3D('',#5820,#4575,#4576);
#4060=AXIS2_PLACEMENT_3D('',#5829,#4582,#4583);
#4061=AXIS2_PLACEMENT_3D('',#5843,#4592,#4593);
#4062=AXIS2_PLACEMENT_3D('',#5850,#4598,#4599);
#4063=AXIS2_PLACEMENT_3D('',#5852,#4600,#4601);
#4064=AXIS2_PLACEMENT_3D('',#5854,#4602,#4603);
#4065=AXIS2_PLACEMENT_3D('',#5855,#4604,#4605);
#4066=AXIS2_PLACEMENT_3D('',#5864,#4611,#4612);
#4067=AXIS2_PLACEMENT_3D('',#5866,#4613,#4614);
#4068=AXIS2_PLACEMENT_3D('',#5868,#4616,#4617);
#4069=AXIS2_PLACEMENT_3D('',#5872,#4619,#4620);
#4070=AXIS2_PLACEMENT_3D('',#5880,#4625,#4626);
#4071=AXIS2_PLACEMENT_3D('',#5883,#4627,#4628);
#4072=AXIS2_PLACEMENT_3D('',#5894,#4635,#4636);
#4073=AXIS2_PLACEMENT_3D('',#5896,#4638,#4639);
#4074=AXIS2_PLACEMENT_3D('',#5897,#4640,#4641);
#4075=AXIS2_PLACEMENT_3D('',#5905,#4646,#4647);
#4076=AXIS2_PLACEMENT_3D('',#5914,#4653,#4654);
#4077=AXIS2_PLACEMENT_3D('',#5917,#4656,#4657);
#4078=AXIS2_PLACEMENT_3D('',#5918,#4658,#4659);
#4079=AXIS2_PLACEMENT_3D('',#5921,#4660,#4661);
#4080=AXIS2_PLACEMENT_3D('',#5930,#4667,#4668);
#4081=AXIS2_PLACEMENT_3D('',#5939,#4674,#4675);
#4082=AXIS2_PLACEMENT_3D('',#5945,#4678,#4679);
#4083=AXIS2_PLACEMENT_3D('',#5953,#4684,#4685);
#4084=AXIS2_PLACEMENT_3D('',#5954,#4686,#4687);
#4085=AXIS2_PLACEMENT_3D('',#5955,#4688,#4689);
#4086=AXIS2_PLACEMENT_3D('',#5958,#4692,#4693);
#4087=AXIS2_PLACEMENT_3D('',#5960,#4695,#4696);
#4088=AXIS2_PLACEMENT_3D('',#5962,#4698,#4699);
#4089=AXIS2_PLACEMENT_3D('',#5963,#4700,#4701);
#4090=AXIS2_PLACEMENT_3D('',#5966,#4704,#4705);
#4091=AXIS2_PLACEMENT_3D('',#5968,#4707,#4708);
#4092=AXIS2_PLACEMENT_3D('',#5970,#4710,#4711);
#4093=AXIS2_PLACEMENT_3D('',#5971,#4712,#4713);
#4094=AXIS2_PLACEMENT_3D('',#5973,#4715,#4716);
#4095=AXIS2_PLACEMENT_3D('',#5975,#4718,#4719);
#4096=AXIS2_PLACEMENT_3D('',#5977,#4721,#4722);
#4097=AXIS2_PLACEMENT_3D('',#5979,#4724,#4725);
#4098=AXIS2_PLACEMENT_3D('',#5985,#4728,#4729);
#4099=AXIS2_PLACEMENT_3D('',#5993,#4734,#4735);
#4100=AXIS2_PLACEMENT_3D('',#5996,#4737,#4738);
#4101=AXIS2_PLACEMENT_3D('',#5997,#4739,#4740);
#4102=AXIS2_PLACEMENT_3D('',#5998,#4741,#4742);
#4103=AXIS2_PLACEMENT_3D('',#6001,#4743,#4744);
#4104=AXIS2_PLACEMENT_3D('',#6010,#4750,#4751);
#4105=AXIS2_PLACEMENT_3D('',#6016,#4754,#4755);
#4106=AXIS2_PLACEMENT_3D('',#6024,#4760,#4761);
#4107=AXIS2_PLACEMENT_3D('',#6027,#4763,#4764);
#4108=AXIS2_PLACEMENT_3D('',#6028,#4765,#4766);
#4109=AXIS2_PLACEMENT_3D('',#6029,#4767,#4768);
#4110=AXIS2_PLACEMENT_3D('',#6032,#4769,#4770);
#4111=AXIS2_PLACEMENT_3D('',#6041,#4776,#4777);
#4112=AXIS2_PLACEMENT_3D('',#6047,#4781,#4782);
#4113=AXIS2_PLACEMENT_3D('',#6051,#4785,#4786);
#4114=AXIS2_PLACEMENT_3D('',#6053,#4788,#4789);
#4115=AXIS2_PLACEMENT_3D('',#6056,#4792,#4793);
#4116=AXIS2_PLACEMENT_3D('',#6069,#4800,#4801);
#4117=AXIS2_PLACEMENT_3D('',#6070,#4802,#4803);
#4118=AXIS2_PLACEMENT_3D('',#6074,#4806,#4807);
#4119=AXIS2_PLACEMENT_3D('',#6080,#4811,#4812);
#4120=AXIS2_PLACEMENT_3D('',#6083,#4815,#4816);
#4121=AXIS2_PLACEMENT_3D('',#6085,#4818,#4819);
#4122=AXIS2_PLACEMENT_3D('',#6098,#4826,#4827);
#4123=AXIS2_PLACEMENT_3D('',#6099,#4828,#4829);
#4124=AXIS2_PLACEMENT_3D('',#6103,#4832,#4833);
#4125=AXIS2_PLACEMENT_3D('',#6109,#4837,#4838);
#4126=AXIS2_PLACEMENT_3D('',#6112,#4841,#4842);
#4127=AXIS2_PLACEMENT_3D('',#6114,#4844,#4845);
#4128=AXIS2_PLACEMENT_3D('',#6127,#4852,#4853);
#4129=AXIS2_PLACEMENT_3D('',#6128,#4854,#4855);
#4130=AXIS2_PLACEMENT_3D('',#6132,#4858,#4859);
#4131=AXIS2_PLACEMENT_3D('',#6138,#4863,#4864);
#4132=AXIS2_PLACEMENT_3D('',#6141,#4867,#4868);
#4133=AXIS2_PLACEMENT_3D('',#6143,#4870,#4871);
#4134=AXIS2_PLACEMENT_3D('',#6156,#4878,#4879);
#4135=AXIS2_PLACEMENT_3D('',#6157,#4880,#4881);
#4136=AXIS2_PLACEMENT_3D('',#6159,#4883,#4884);
#4137=AXIS2_PLACEMENT_3D('',#6162,#4887,#4888);
#4138=AXIS2_PLACEMENT_3D('',#6163,#4889,#4890);
#4139=AXIS2_PLACEMENT_3D('',#6164,#4891,#4892);
#4140=AXIS2_PLACEMENT_3D('',#6167,#4895,#4896);
#4141=AXIS2_PLACEMENT_3D('',#6169,#4898,#4899);
#4142=AXIS2_PLACEMENT_3D('',#6170,#4900,#4901);
#4143=AXIS2_PLACEMENT_3D('',#6171,#4902,#4903);
#4144=AXIS2_PLACEMENT_3D('',#6172,#4904,#4905);
#4145=AXIS2_PLACEMENT_3D('',#6173,#4906,#4907);
#4146=AXIS2_PLACEMENT_3D('',#6174,#4908,#4909);
#4147=AXIS2_PLACEMENT_3D('',#6175,#4910,#4911);
#4148=AXIS2_PLACEMENT_3D('',#6176,#4912,#4913);
#4149=AXIS2_PLACEMENT_3D('',#6177,#4914,#4915);
#4150=AXIS2_PLACEMENT_3D('',#6178,#4916,#4917);
#4151=AXIS2_PLACEMENT_3D('',#6179,#4918,#4919);
#4152=AXIS2_PLACEMENT_3D('',#6180,#4920,#4921);
#4153=AXIS2_PLACEMENT_3D('',#6181,#4922,#4923);
#4154=AXIS2_PLACEMENT_3D('',#6182,#4924,#4925);
#4155=AXIS2_PLACEMENT_3D('',#6183,#4926,#4927);
#4156=AXIS2_PLACEMENT_3D('',#6184,#4928,#4929);
#4157=AXIS2_PLACEMENT_3D('',#6185,#4930,#4931);
#4158=AXIS2_PLACEMENT_3D('',#6186,#4932,#4933);
#4159=AXIS2_PLACEMENT_3D('',#6187,#4934,#4935);
#4160=AXIS2_PLACEMENT_3D('',#6188,#4936,#4937);
#4161=AXIS2_PLACEMENT_3D('',#6189,#4938,#4939);
#4162=AXIS2_PLACEMENT_3D('',#6190,#4940,#4941);
#4163=AXIS2_PLACEMENT_3D('',#6191,#4942,#4943);
#4164=AXIS2_PLACEMENT_3D('',#6192,#4944,#4945);
#4165=AXIS2_PLACEMENT_3D('',#6193,#4946,#4947);
#4166=AXIS2_PLACEMENT_3D('',#6194,#4948,#4949);
#4167=AXIS2_PLACEMENT_3D('',#6195,#4950,#4951);
#4168=AXIS2_PLACEMENT_3D('',#6196,#4952,#4953);
#4169=AXIS2_PLACEMENT_3D('',#6197,#4954,#4955);
#4170=AXIS2_PLACEMENT_3D('',#6198,#4956,#4957);
#4171=AXIS2_PLACEMENT_3D('',#6199,#4958,#4959);
#4172=AXIS2_PLACEMENT_3D('',#6200,#4960,#4961);
#4173=AXIS2_PLACEMENT_3D('',#6201,#4962,#4963);
#4174=AXIS2_PLACEMENT_3D('',#6202,#4964,#4965);
#4175=AXIS2_PLACEMENT_3D('',#6203,#4966,#4967);
#4176=AXIS2_PLACEMENT_3D('',#6204,#4968,#4969);
#4177=AXIS2_PLACEMENT_3D('',#6205,#4970,#4971);
#4178=AXIS2_PLACEMENT_3D('',#6206,#4972,#4973);
#4179=AXIS2_PLACEMENT_3D('',#6207,#4974,#4975);
#4180=AXIS2_PLACEMENT_3D('',#6208,#4976,#4977);
#4181=AXIS2_PLACEMENT_3D('',#6209,#4978,#4979);
#4182=AXIS2_PLACEMENT_3D('',#6210,#4980,#4981);
#4183=AXIS2_PLACEMENT_3D('',#6211,#4982,#4983);
#4184=AXIS2_PLACEMENT_3D('',#6212,#4984,#4985);
#4185=AXIS2_PLACEMENT_3D('',#6213,#4986,#4987);
#4186=AXIS2_PLACEMENT_3D('',#6214,#4988,#4989);
#4187=AXIS2_PLACEMENT_3D('',#6215,#4990,#4991);
#4188=AXIS2_PLACEMENT_3D('',#6216,#4992,#4993);
#4189=AXIS2_PLACEMENT_3D('',#6217,#4994,#4995);
#4190=AXIS2_PLACEMENT_3D('',#6218,#4996,#4997);
#4191=AXIS2_PLACEMENT_3D('',#6219,#4998,#4999);
#4192=AXIS2_PLACEMENT_3D('',#6220,#5000,#5001);
#4193=AXIS2_PLACEMENT_3D('',#6221,#5002,#5003);
#4194=AXIS2_PLACEMENT_3D('',#6222,#5004,#5005);
#4195=AXIS2_PLACEMENT_3D('',#6223,#5006,#5007);
#4196=AXIS2_PLACEMENT_3D('',#6224,#5008,#5009);
#4197=AXIS2_PLACEMENT_3D('',#6225,#5010,#5011);
#4198=AXIS2_PLACEMENT_3D('',#6226,#5012,#5013);
#4199=AXIS2_PLACEMENT_3D('',#6227,#5014,#5015);
#4200=AXIS2_PLACEMENT_3D('',#6228,#5016,#5017);
#4201=AXIS2_PLACEMENT_3D('',#6229,#5018,#5019);
#4202=AXIS2_PLACEMENT_3D('',#6230,#5020,#5021);
#4203=AXIS2_PLACEMENT_3D('',#6231,#5022,#5023);
#4204=AXIS2_PLACEMENT_3D('',#6232,#5024,#5025);
#4205=AXIS2_PLACEMENT_3D('',#6233,#5026,#5027);
#4206=AXIS2_PLACEMENT_3D('',#6234,#5028,#5029);
#4207=AXIS2_PLACEMENT_3D('',#6235,#5030,#5031);
#4208=AXIS2_PLACEMENT_3D('',#6236,#5032,#5033);
#4209=AXIS2_PLACEMENT_3D('',#6237,#5034,#5035);
#4210=AXIS2_PLACEMENT_3D('',#6238,#5036,#5037);
#4211=AXIS2_PLACEMENT_3D('',#6239,#5038,#5039);
#4212=AXIS2_PLACEMENT_3D('',#6240,#5040,#5041);
#4213=AXIS2_PLACEMENT_3D('',#6241,#5042,#5043);
#4214=AXIS2_PLACEMENT_3D('',#6242,#5044,#5045);
#4215=AXIS2_PLACEMENT_3D('',#6243,#5046,#5047);
#4216=AXIS2_PLACEMENT_3D('',#6244,#5048,#5049);
#4217=AXIS2_PLACEMENT_3D('',#6245,#5050,#5051);
#4218=AXIS2_PLACEMENT_3D('',#6246,#5052,#5053);
#4219=AXIS2_PLACEMENT_3D('',#6247,#5054,#5055);
#4220=AXIS2_PLACEMENT_3D('',#6248,#5056,#5057);
#4221=AXIS2_PLACEMENT_3D('',#6249,#5058,#5059);
#4222=AXIS2_PLACEMENT_3D('',#6250,#5060,#5061);
#4223=AXIS2_PLACEMENT_3D('',#6251,#5062,#5063);
#4224=AXIS2_PLACEMENT_3D('',#6253,#5065,#5066);
#4225=AXIS2_PLACEMENT_3D('',#6255,#5068,#5069);
#4226=AXIS2_PLACEMENT_3D('',#6256,#5070,#5071);
#4227=AXIS2_PLACEMENT_3D('',#6265,#5076,#5077);
#4228=AXIS2_PLACEMENT_3D('',#6271,#5081,#5082);
#4229=AXIS2_PLACEMENT_3D('',#6277,#5086,#5087);
#4230=AXIS2_PLACEMENT_3D('',#6280,#5090,#5091);
#4231=AXIS2_PLACEMENT_3D('',#6283,#5092,#5093);
#4232=AXIS2_PLACEMENT_3D('',#6287,#5095,#5096);
#4233=AXIS2_PLACEMENT_3D('',#6291,#5098,#5099);
#4234=AXIS2_PLACEMENT_3D('',#6295,#5101,#5102);
#4235=AXIS2_PLACEMENT_3D('',#6299,#5104,#5105);
#4236=AXIS2_PLACEMENT_3D('',#6303,#5107,#5108);
#4237=AXIS2_PLACEMENT_3D('',#6307,#5110,#5111);
#4238=AXIS2_PLACEMENT_3D('',#6311,#5113,#5114);
#4239=AXIS2_PLACEMENT_3D('',#6315,#5116,#5117);
#4240=AXIS2_PLACEMENT_3D('',#6319,#5119,#5120);
#4241=AXIS2_PLACEMENT_3D('',#6322,#5122,#5123);
#4242=AXIS2_PLACEMENT_3D('',#6324,#5124,#5125);
#4243=AXIS2_PLACEMENT_3D('',#6326,#5126,#5127);
#4244=AXIS2_PLACEMENT_3D('',#6328,#5128,#5129);
#4245=AXIS2_PLACEMENT_3D('',#6329,#5130,#5131);
#4246=AXIS2_PLACEMENT_3D('',#6334,#5133,#5134);
#4247=AXIS2_PLACEMENT_3D('',#6337,#5136,#5137);
#4248=AXIS2_PLACEMENT_3D('',#6342,#5139,#5140);
#4249=AXIS2_PLACEMENT_3D('',#6345,#5142,#5143);
#4250=AXIS2_PLACEMENT_3D('',#6350,#5145,#5146);
#4251=AXIS2_PLACEMENT_3D('',#6353,#5148,#5149);
#4252=AXIS2_PLACEMENT_3D('',#6358,#5151,#5152);
#4253=AXIS2_PLACEMENT_3D('',#6361,#5154,#5155);
#4254=AXIS2_PLACEMENT_3D('',#6366,#5157,#5158);
#4255=AXIS2_PLACEMENT_3D('',#6369,#5160,#5161);
#4256=AXIS2_PLACEMENT_3D('',#6371,#5162,#5163);
#4257=AXIS2_PLACEMENT_3D('',#6373,#5164,#5165);
#4258=AXIS2_PLACEMENT_3D('',#6375,#5166,#5167);
#4259=AXIS2_PLACEMENT_3D('',#6377,#5168,#5169);
#4260=AXIS2_PLACEMENT_3D('',#6378,#5170,#5171);
#4261=AXIS2_PLACEMENT_3D('',#6380,#5173,#5174);
#4262=AXIS2_PLACEMENT_3D('',#6382,#5176,#5177);
#4263=AXIS2_PLACEMENT_3D('',#6384,#5179,#5180);
#4264=AXIS2_PLACEMENT_3D('',#6386,#5182,#5183);
#4265=AXIS2_PLACEMENT_3D('',#6389,#5186,#5187);
#4266=AXIS2_PLACEMENT_3D('',#6391,#5189,#5190);
#4267=AXIS2_PLACEMENT_3D('',#6393,#5192,#5193);
#4268=AXIS2_PLACEMENT_3D('',#6394,#5194,#5195);
#4269=AXIS2_PLACEMENT_3D('',#6397,#5198,#5199);
#4270=AXIS2_PLACEMENT_3D('',#6399,#5201,#5202);
#4271=AXIS2_PLACEMENT_3D('',#6401,#5204,#5205);
#4272=AXIS2_PLACEMENT_3D('',#6402,#5206,#5207);
#4273=AXIS2_PLACEMENT_3D('',#6405,#5210,#5211);
#4274=AXIS2_PLACEMENT_3D('',#6407,#5213,#5214);
#4275=AXIS2_PLACEMENT_3D('',#6409,#5216,#5217);
#4276=AXIS2_PLACEMENT_3D('',#6410,#5218,#5219);
#4277=AXIS2_PLACEMENT_3D('',#6413,#5222,#5223);
#4278=AXIS2_PLACEMENT_3D('',#6415,#5225,#5226);
#4279=AXIS2_PLACEMENT_3D('',#6417,#5228,#5229);
#4280=AXIS2_PLACEMENT_3D('',#6418,#5230,#5231);
#4281=AXIS2_PLACEMENT_3D('',#6421,#5234,#5235);
#4282=AXIS2_PLACEMENT_3D('',#6423,#5237,#5238);
#4283=AXIS2_PLACEMENT_3D('',#6425,#5240,#5241);
#4284=AXIS2_PLACEMENT_3D('',#6426,#5242,#5243);
#4285=AXIS2_PLACEMENT_3D('',#6427,#5244,#5245);
#4286=AXIS2_PLACEMENT_3D('',#6428,#5246,#5247);
#4287=AXIS2_PLACEMENT_3D('',#6429,#5248,#5249);
#4288=AXIS2_PLACEMENT_3D('',#6430,#5250,#5251);
#4289=AXIS2_PLACEMENT_3D('',#6432,#5252,#5253);
#4290=AXIS2_PLACEMENT_3D('',#6436,#5255,#5256);
#4291=AXIS2_PLACEMENT_3D('',#6440,#5258,#5259);
#4292=AXIS2_PLACEMENT_3D('',#6444,#5261,#5262);
#4293=AXIS2_PLACEMENT_3D('',#6448,#5264,#5265);
#4294=AXIS2_PLACEMENT_3D('',#6451,#5267,#5268);
#4295=AXIS2_PLACEMENT_3D('',#6452,#5269,#5270);
#4296=AXIS2_PLACEMENT_3D('',#6464,#5277,#5278);
#4297=AXIS2_PLACEMENT_3D('',#6465,#5279,#5280);
#4298=AXIS2_PLACEMENT_3D('',#6466,#5281,#5282);
#4299=AXIS2_PLACEMENT_3D('',#6472,#5286,#5287);
#4300=AXIS2_PLACEMENT_3D('',#6474,#5289,#5290);
#4301=AXIS2_PLACEMENT_3D('',#6476,#5292,#5293);
#4302=AXIS2_PLACEMENT_3D('',#6477,#5294,#5295);
#4303=AXIS2_PLACEMENT_3D('',#6483,#5299,#5300);
#4304=AXIS2_PLACEMENT_3D('',#6485,#5302,#5303);
#4305=AXIS2_PLACEMENT_3D('',#6487,#5305,#5306);
#4306=AXIS2_PLACEMENT_3D('',#6488,#5307,#5308);
#4307=AXIS2_PLACEMENT_3D('',#6490,#5309,#5310);
#4308=AXIS2_PLACEMENT_3D('',#6492,#5312,#5313);
#4309=AXIS2_PLACEMENT_3D('',#6493,#5314,#5315);
#4310=AXIS2_PLACEMENT_3D('',#6494,#5316,#5317);
#4311=AXIS2_PLACEMENT_3D('',#6497,#5318,#5319);
#4312=AXIS2_PLACEMENT_3D('',#6499,#5320,#5321);
#4313=AXIS2_PLACEMENT_3D('',#6501,#5322,#5323);
#4314=AXIS2_PLACEMENT_3D('',#6502,#5324,#5325);
#4315=AXIS2_PLACEMENT_3D('',#6503,#5326,#5327);
#4316=AXIS2_PLACEMENT_3D('',#6504,#5328,#5329);
#4317=AXIS2_PLACEMENT_3D('',#6506,#5330,#5331);
#4318=AXIS2_PLACEMENT_3D('',#6508,#5333,#5334);
#4319=AXIS2_PLACEMENT_3D('',#6511,#5335,#5336);
#4320=AXIS2_PLACEMENT_3D('',#6512,#5337,#5338);
#4321=AXIS2_PLACEMENT_3D('',#6515,#5340,#5341);
#4322=AXIS2_PLACEMENT_3D('',#6516,#5342,#5343);
#4323=AXIS2_PLACEMENT_3D('',#6518,#5344,#5345);
#4324=AXIS2_PLACEMENT_3D('',#6519,#5346,#5347);
#4325=AXIS2_PLACEMENT_3D('',#6521,#5348,#5349);
#4326=AXIS2_PLACEMENT_3D('',#6522,#5350,#5351);
#4327=AXIS2_PLACEMENT_3D('',#6523,#5352,#5353);
#4328=AXIS2_PLACEMENT_3D('',#6525,#5354,#5355);
#4329=AXIS2_PLACEMENT_3D('',#6527,#5357,#5358);
#4330=AXIS2_PLACEMENT_3D('',#6529,#5359,#5360);
#4331=AXIS2_PLACEMENT_3D('',#6530,#5361,#5362);
#4332=AXIS2_PLACEMENT_3D('',#6531,#5363,#5364);
#4333=AXIS2_PLACEMENT_3D('',#6532,#5365,#5366);
#4334=AXIS2_PLACEMENT_3D('',#6534,#5367,#5368);
#4335=AXIS2_PLACEMENT_3D('',#6536,#5369,#5370);
#4336=AXIS2_PLACEMENT_3D('',#6537,#5371,#5372);
#4337=AXIS2_PLACEMENT_3D('',#6538,#5373,#5374);
#4338=AXIS2_PLACEMENT_3D('',#6541,#5376,#5377);
#4339=AXIS2_PLACEMENT_3D('',#6542,#5378,#5379);
#4340=AXIS2_PLACEMENT_3D('',#6544,#5380,#5381);
#4341=AXIS2_PLACEMENT_3D('',#6546,#5383,#5384);
#4342=AXIS2_PLACEMENT_3D('',#6548,#5385,#5386);
#4343=AXIS2_PLACEMENT_3D('',#6549,#5387,#5388);
#4344=AXIS2_PLACEMENT_3D('',#6551,#5389,#5390);
#4345=AXIS2_PLACEMENT_3D('',#6552,#5391,#5392);
#4346=AXIS2_PLACEMENT_3D('',#6553,#5393,#5394);
#4347=AXIS2_PLACEMENT_3D('',#6556,#5396,#5397);
#4348=AXIS2_PLACEMENT_3D('',#6557,#5398,#5399);
#4349=AXIS2_PLACEMENT_3D('',#6559,#5400,#5401);
#4350=AXIS2_PLACEMENT_3D('',#6560,#5402,#5403);
#4351=AXIS2_PLACEMENT_3D('',#6561,#5404,#5405);
#4352=AXIS2_PLACEMENT_3D('',#6562,#5406,#5407);
#4353=AXIS2_PLACEMENT_3D('',#6563,#5408,#5409);
#4354=AXIS2_PLACEMENT_3D('',#6565,#5410,#5411);
#4355=AXIS2_PLACEMENT_3D('',#6568,#5413,#5414);
#4356=AXIS2_PLACEMENT_3D('',#6569,#5415,#5416);
#4357=AXIS2_PLACEMENT_3D('',#6572,#5417,#5418);
#4358=AXIS2_PLACEMENT_3D('',#6573,#5419,#5420);
#4359=AXIS2_PLACEMENT_3D('',#6576,#5422,#5423);
#4360=AXIS2_PLACEMENT_3D('',#6577,#5424,#5425);
#4361=AXIS2_PLACEMENT_3D('',#6579,#5426,#5427);
#4362=AXIS2_PLACEMENT_3D('',#6582,#5429,#5430);
#4363=AXIS2_PLACEMENT_3D('',#6583,#5431,#5432);
#4364=AXIS2_PLACEMENT_3D('',#6585,#5433,#5434);
#4365=AXIS2_PLACEMENT_3D('',#6588,#5436,#5437);
#4366=AXIS2_PLACEMENT_3D('',#6589,#5438,#5439);
#4367=AXIS2_PLACEMENT_3D('',#6591,#5440,#5441);
#4368=AXIS2_PLACEMENT_3D('',#6594,#5443,#5444);
#4369=AXIS2_PLACEMENT_3D('',#6595,#5445,#5446);
#4370=AXIS2_PLACEMENT_3D('',#6597,#5447,#5448);
#4371=AXIS2_PLACEMENT_3D('',#6600,#5450,#5451);
#4372=AXIS2_PLACEMENT_3D('',#6601,#5452,#5453);
#4373=AXIS2_PLACEMENT_3D('',#6603,#5454,#5455);
#4374=AXIS2_PLACEMENT_3D('',#6606,#5457,#5458);
#4375=AXIS2_PLACEMENT_3D('',#6607,#5459,#5460);
#4376=AXIS2_PLACEMENT_3D('',#6609,#5461,#5462);
#4377=AXIS2_PLACEMENT_3D('',#6612,#5464,#5465);
#4378=AXIS2_PLACEMENT_3D('',#6613,#5466,#5467);
#4379=AXIS2_PLACEMENT_3D('',#6615,#5468,#5469);
#4380=AXIS2_PLACEMENT_3D('',#6618,#5471,#5472);
#4381=AXIS2_PLACEMENT_3D('',#6619,#5473,#5474);
#4382=AXIS2_PLACEMENT_3D('',#6620,#5475,#5476);
#4383=AXIS2_PLACEMENT_3D('',#6621,#5477,#5478);
#4384=AXIS2_PLACEMENT_3D('',#6623,#5479,#5480);
#4385=AXIS2_PLACEMENT_3D('',#6625,#5481,#5482);
#4386=AXIS2_PLACEMENT_3D('',#6626,#5483,#5484);
#4387=AXIS2_PLACEMENT_3D('',#6628,#5485,#5486);
#4388=AXIS2_PLACEMENT_3D('',#6630,#5487,#5488);
#4389=AXIS2_PLACEMENT_3D('',#6631,#5489,#5490);
#4390=AXIS2_PLACEMENT_3D('',#6633,#5491,#5492);
#4391=AXIS2_PLACEMENT_3D('',#6635,#5494,#5495);
#4392=AXIS2_PLACEMENT_3D('',#6637,#5496,#5497);
#4393=AXIS2_PLACEMENT_3D('',#6640,#5499,#5500);
#4394=AXIS2_PLACEMENT_3D('',#6641,#5501,#5502);
#4395=AXIS2_PLACEMENT_3D('',#6644,#5504,#5505);
#4396=AXIS2_PLACEMENT_3D('',#6645,#5506,#5507);
#4397=AXIS2_PLACEMENT_3D('',#6646,#5508,#5509);
#4398=AXIS2_PLACEMENT_3D('',#6647,#5510,#5511);
#4399=AXIS2_PLACEMENT_3D('',#6649,#5513,#5514);
#4400=AXIS2_PLACEMENT_3D('',#6653,#5516,#5517);
#4401=AXIS2_PLACEMENT_3D('',#6654,#5518,#5519);
#4402=AXIS2_PLACEMENT_3D('',#6655,#5520,#5521);
#4403=AXIS2_PLACEMENT_3D('',#6658,#5523,#5524);
#4404=AXIS2_PLACEMENT_3D('',#6659,#5525,#5526);
#4405=AXIS2_PLACEMENT_3D('',#6661,#5528,#5529);
#4406=AXIS2_PLACEMENT_3D('',#6662,#5530,#5531);
#4407=AXIS2_PLACEMENT_3D('',#6671,#5536,#5537);
#4408=AXIS2_PLACEMENT_3D('',#6677,#5541,#5542);
#4409=AXIS2_PLACEMENT_3D('',#6683,#5546,#5547);
#4410=AXIS2_PLACEMENT_3D('',#6685,#5548,#5549);
#4411=AXIS2_PLACEMENT_3D('',#6688,#5551,#5552);
#4412=AXIS2_PLACEMENT_3D('',#6698,#5553,#5554);
#4413=AXIS2_PLACEMENT_3D('',#6700,#5556,#5557);
#4414=AXIS2_PLACEMENT_3D('',#6702,#5558,#5559);
#4415=AXIS2_PLACEMENT_3D('',#6714,#5563,#5564);
#4416=AXIS2_PLACEMENT_3D('',#6720,#5568,#5569);
#4417=AXIS2_PLACEMENT_3D('',#6724,#5572,#5573);
#4418=AXIS2_PLACEMENT_3D('',#6728,#5576,#5577);
#4419=AXIS2_PLACEMENT_3D('',#6730,#5579,#5580);
#4420=AXIS2_PLACEMENT_3D('',#6731,#5581,#5582);
#4421=AXIS2_PLACEMENT_3D('',#6732,#5583,#5584);
#4422=AXIS2_PLACEMENT_3D('',#6747,#5585,#5586);
#4423=AXIS2_PLACEMENT_3D('',#6748,#5587,#5588);
#4424=AXIS2_PLACEMENT_3D('',#6749,#5589,#5590);
#4425=AXIS2_PLACEMENT_3D('',#6765,#5592,#5593);
#4426=AXIS2_PLACEMENT_3D('',#6766,#5594,#5595);
#4427=AXIS2_PLACEMENT_3D('',#6767,#5596,#5597);
#4428=AXIS2_PLACEMENT_3D('',#6768,#5598,#5599);
#4429=AXIS2_PLACEMENT_3D('',#6769,#5600,#5601);
#4430=AXIS2_PLACEMENT_3D('',#6770,#5602,#5603);
#4431=AXIS2_PLACEMENT_3D('',#6771,#5604,#5605);
#4432=DIRECTION('axis',(0.,0.,1.));
#4433=DIRECTION('refdir',(1.,0.,0.));
#4434=DIRECTION('axis',(0.,0.,1.));
#4435=DIRECTION('refdir',(1.,0.,0.));
#4436=DIRECTION('axis',(0.,0.,1.));
#4437=DIRECTION('refdir',(1.,0.,0.));
#4438=DIRECTION('center_axis',(0.,0.,1.));
#4439=DIRECTION('ref_axis',(1.,0.,0.));
#4440=DIRECTION('',(-1.,0.,0.));
#4441=DIRECTION('',(0.,1.,0.));
#4442=DIRECTION('',(1.,0.,0.));
#4443=DIRECTION('',(0.,1.,0.));
#4444=DIRECTION('',(1.,0.,0.));
#4445=DIRECTION('',(0.,1.,0.));
#4446=DIRECTION('',(1.,0.,0.));
#4447=DIRECTION('',(0.,-1.,0.));
#4448=DIRECTION('',(-1.,0.,0.));
#4449=DIRECTION('',(0.,1.,0.));
#4450=DIRECTION('',(1.,0.,0.));
#4451=DIRECTION('',(0.,-1.,0.));
#4452=DIRECTION('center_axis',(0.,0.,1.));
#4453=DIRECTION('ref_axis',(1.,0.,0.));
#4454=DIRECTION('center_axis',(0.,0.,1.));
#4455=DIRECTION('ref_axis',(1.,0.,0.));
#4456=DIRECTION('center_axis',(0.,0.,1.));
#4457=DIRECTION('ref_axis',(1.,0.,0.));
#4458=DIRECTION('center_axis',(0.,0.,1.));
#4459=DIRECTION('ref_axis',(1.,0.,0.));
#4460=DIRECTION('',(1.14603667058081E-16,-1.,0.));
#4461=DIRECTION('',(1.,0.,0.));
#4462=DIRECTION('',(-2.29207334116161E-16,-1.,0.));
#4463=DIRECTION('',(1.,0.,0.));
#4464=DIRECTION('',(-1.,0.,0.));
#4465=DIRECTION('',(0.,-1.,0.));
#4466=DIRECTION('',(-1.,0.,0.));
#4467=DIRECTION('',(0.,-1.,0.));
#4468=DIRECTION('center_axis',(1.,0.,1.85037170770859E-16));
#4469=DIRECTION('ref_axis',(1.85037170770859E-16,0.,-1.));
#4470=DIRECTION('',(0.,1.,0.));
#4471=DIRECTION('',(-2.83084755282908E-16,2.83084755282908E-16,1.));
#4472=DIRECTION('',(0.,-1.,0.));
#4473=DIRECTION('',(0.,0.,1.));
#4474=DIRECTION('',(2.368475785867E-16,0.,-1.));
#4475=DIRECTION('',(0.,1.,0.));
#4476=DIRECTION('',(0.,0.,1.));
#4477=DIRECTION('center_axis',(0.,0.,1.));
#4478=DIRECTION('ref_axis',(1.,0.,0.));
#4479=DIRECTION('',(-1.,0.,0.));
#4480=DIRECTION('',(0.,-1.,0.));
#4481=DIRECTION('',(-1.,0.,0.));
#4482=DIRECTION('',(1.,0.,0.));
#4483=DIRECTION('',(0.,1.,0.));
#4484=DIRECTION('',(-1.,0.,0.));
#4485=DIRECTION('',(0.,1.,0.));
#4486=DIRECTION('',(-1.,0.,0.));
#4487=DIRECTION('',(0.,-1.,0.));
#4488=DIRECTION('',(-1.,0.,0.));
#4489=DIRECTION('',(0.,1.,0.));
#4490=DIRECTION('center_axis',(1.,0.,0.));
#4491=DIRECTION('ref_axis',(0.,0.,-1.));
#4492=DIRECTION('',(0.,-2.83084755282908E-16,-1.));
#4493=DIRECTION('',(0.,-1.,0.));
#4494=DIRECTION('',(0.,0.,-1.));
#4495=DIRECTION('',(0.,0.,-1.));
#4496=DIRECTION('',(0.,0.,-1.));
#4497=DIRECTION('',(0.,1.,0.));
#4498=DIRECTION('center_axis',(0.,-1.,0.));
#4499=DIRECTION('ref_axis',(0.,0.,-1.));
#4500=DIRECTION('',(1.,0.,0.));
#4501=DIRECTION('',(0.,0.,-1.));
#4502=DIRECTION('',(1.,0.,0.));
#4503=DIRECTION('',(0.,0.,-1.));
#4504=DIRECTION('',(1.,0.,0.));
#4505=DIRECTION('',(0.,0.,-1.));
#4506=DIRECTION('center_axis',(0.,-1.,0.));
#4507=DIRECTION('ref_axis',(0.,0.,-1.));
#4508=DIRECTION('',(1.,0.,0.));
#4509=DIRECTION('',(0.,0.,-1.));
#4510=DIRECTION('',(1.,0.,0.));
#4511=DIRECTION('',(0.,0.,1.));
#4512=DIRECTION('',(1.,0.,0.));
#4513=DIRECTION('',(0.,0.,-1.));
#4514=DIRECTION('center_axis',(0.,0.,1.));
#4515=DIRECTION('ref_axis',(1.,0.,0.));
#4516=DIRECTION('',(-1.,0.,0.));
#4517=DIRECTION('',(0.,-1.,0.));
#4518=DIRECTION('',(1.,0.,0.));
#4519=DIRECTION('',(0.,1.,0.));
#4520=DIRECTION('',(-1.,0.,0.));
#4521=DIRECTION('',(0.,-1.,0.));
#4522=DIRECTION('',(1.,0.,0.));
#4523=DIRECTION('',(0.,1.,0.));
#4524=DIRECTION('',(1.,0.,0.));
#4525=DIRECTION('',(0.,1.,0.));
#4526=DIRECTION('',(1.,0.,0.));
#4527=DIRECTION('',(0.,1.,0.));
#4528=DIRECTION('',(0.,-1.,0.));
#4529=DIRECTION('',(-1.,0.,0.));
#4530=DIRECTION('',(0.,-1.,0.));
#4531=DIRECTION('',(-1.,0.,0.));
#4532=DIRECTION('center_axis',(0.,0.,1.));
#4533=DIRECTION('ref_axis',(1.,0.,0.));
#4534=DIRECTION('center_axis',(0.,0.,1.));
#4535=DIRECTION('ref_axis',(1.,0.,0.));
#4536=DIRECTION('center_axis',(0.,0.,1.));
#4537=DIRECTION('ref_axis',(1.,0.,0.));
#4538=DIRECTION('center_axis',(0.,0.,1.));
#4539=DIRECTION('ref_axis',(1.,0.,0.));
#4540=DIRECTION('',(1.,0.,0.));
#4541=DIRECTION('',(1.14603667058081E-16,-1.,0.));
#4542=DIRECTION('',(1.,0.,0.));
#4543=DIRECTION('',(-2.29207334116161E-16,-1.,0.));
#4544=DIRECTION('center_axis',(0.,-1.,0.));
#4545=DIRECTION('ref_axis',(0.,0.,-1.));
#4546=DIRECTION('',(0.,0.,-1.));
#4547=DIRECTION('',(1.,0.,0.));
#4548=DIRECTION('',(0.,0.,1.));
#4549=DIRECTION('',(1.,0.,0.));
#4550=DIRECTION('center_axis',(0.,-1.,0.));
#4551=DIRECTION('ref_axis',(0.,0.,-1.));
#4552=DIRECTION('',(0.,0.,-1.));
#4553=DIRECTION('',(1.,0.,0.));
#4554=DIRECTION('',(0.,0.,1.));
#4555=DIRECTION('center_axis',(0.,-1.,0.));
#4556=DIRECTION('ref_axis',(0.,0.,-1.));
#4557=DIRECTION('',(-1.,0.,0.));
#4558=DIRECTION('',(0.,0.,-1.));
#4559=DIRECTION('',(0.,0.,-1.));
#4560=DIRECTION('',(1.,0.,0.));
#4561=DIRECTION('',(0.,0.,-1.));
#4562=DIRECTION('center_axis',(0.,-1.,0.));
#4563=DIRECTION('ref_axis',(0.,0.,-1.));
#4564=DIRECTION('',(-1.,0.,0.));
#4565=DIRECTION('',(0.,0.,-1.));
#4566=DIRECTION('',(1.,0.,0.));
#4567=DIRECTION('',(0.,0.,1.));
#4568=DIRECTION('',(0.,0.,-1.));
#4569=DIRECTION('center_axis',(0.,-1.,0.));
#4570=DIRECTION('ref_axis',(0.,0.,-1.));
#4571=DIRECTION('center_axis',(0.,-1.,0.));
#4572=DIRECTION('ref_axis',(0.,0.,-1.));
#4573=DIRECTION('center_axis',(0.,-1.,0.));
#4574=DIRECTION('ref_axis',(0.,0.,-1.));
#4575=DIRECTION('center_axis',(1.,0.,1.85037170770859E-16));
#4576=DIRECTION('ref_axis',(1.85037170770859E-16,0.,-1.));
#4577=DIRECTION('',(0.,1.,0.));
#4578=DIRECTION('',(0.,1.,0.));
#4579=DIRECTION('',(2.39239978370404E-16,0.,-1.));
#4580=DIRECTION('',(0.,-1.,1.18423789293349E-15));
#4581=DIRECTION('',(-2.8421709430404E-16,2.8421709430404E-16,1.));
#4582=DIRECTION('center_axis',(0.,0.,1.));
#4583=DIRECTION('ref_axis',(1.,0.,0.));
#4584=DIRECTION('',(0.,-1.,0.));
#4585=DIRECTION('',(-1.,0.,0.));
#4586=DIRECTION('',(0.,1.,0.));
#4587=DIRECTION('',(0.,1.,0.));
#4588=DIRECTION('',(1.,0.,0.));
#4589=DIRECTION('',(0.,-1.,0.));
#4590=DIRECTION('',(-1.,0.,0.));
#4591=DIRECTION('',(0.,1.,0.));
#4592=DIRECTION('center_axis',(1.,0.,0.));
#4593=DIRECTION('ref_axis',(0.,0.,-1.));
#4594=DIRECTION('',(0.,1.,0.));
#4595=DIRECTION('',(0.,2.8421709430404E-16,1.));
#4596=DIRECTION('',(0.,-1.,0.));
#4597=DIRECTION('',(0.,0.,-1.));
#4598=DIRECTION('center_axis',(0.,-1.,0.));
#4599=DIRECTION('ref_axis',(0.,0.,-1.));
#4600=DIRECTION('center_axis',(0.,-1.,0.));
#4601=DIRECTION('ref_axis',(0.,0.,-1.));
#4602=DIRECTION('center_axis',(0.,-1.,0.));
#4603=DIRECTION('ref_axis',(0.,0.,-1.));
#4604=DIRECTION('center_axis',(1.,0.,0.));
#4605=DIRECTION('ref_axis',(0.,0.,-1.));
#4606=DIRECTION('',(0.,-1.,0.));
#4607=DIRECTION('',(0.,0.,-1.));
#4608=DIRECTION('',(0.,-1.,0.));
#4609=DIRECTION('',(0.,0.,-1.));
#4610=DIRECTION('',(0.,0.,1.));
#4611=DIRECTION('center_axis',(0.,1.,0.));
#4612=DIRECTION('ref_axis',(0.,0.,1.));
#4613=DIRECTION('center_axis',(0.,1.,0.));
#4614=DIRECTION('ref_axis',(0.,0.,1.));
#4615=DIRECTION('',(0.,0.,1.));
#4616=DIRECTION('center_axis',(-1.,0.,0.));
#4617=DIRECTION('ref_axis',(0.,0.,1.));
#4618=DIRECTION('',(0.,-1.,0.));
#4619=DIRECTION('center_axis',(-1.,0.,0.));
#4620=DIRECTION('ref_axis',(0.,0.,1.));
#4621=DIRECTION('',(0.,0.,1.));
#4622=DIRECTION('',(0.,-1.,0.));
#4623=DIRECTION('',(0.,0.,1.));
#4624=DIRECTION('',(0.,-1.,0.));
#4625=DIRECTION('center_axis',(1.,0.,0.));
#4626=DIRECTION('ref_axis',(0.,0.,-1.));
#4627=DIRECTION('center_axis',(1.,0.,0.));
#4628=DIRECTION('ref_axis',(0.,0.,-1.));
#4629=DIRECTION('',(0.,1.,0.));
#4630=DIRECTION('',(0.,0.,1.));
#4631=DIRECTION('',(0.,-1.,0.));
#4632=DIRECTION('',(0.,0.,-1.));
#4633=DIRECTION('',(0.,-1.,0.));
#4634=DIRECTION('',(0.,0.,-1.));
#4635=DIRECTION('center_axis',(0.,1.,0.));
#4636=DIRECTION('ref_axis',(0.,0.,1.));
#4637=DIRECTION('',(0.,0.,1.));
#4638=DIRECTION('center_axis',(0.,1.,0.));
#4639=DIRECTION('ref_axis',(0.,0.,1.));
#4640=DIRECTION('center_axis',(-1.,0.,0.));
#4641=DIRECTION('ref_axis',(0.,0.,1.));
#4642=DIRECTION('',(-3.86108475418265E-15,0.,1.));
#4643=DIRECTION('',(0.,-1.,0.));
#4644=DIRECTION('',(-3.86108475418265E-15,0.,1.));
#4645=DIRECTION('',(0.,-1.,0.));
#4646=DIRECTION('center_axis',(1.,0.,0.));
#4647=DIRECTION('ref_axis',(0.,0.,-1.));
#4648=DIRECTION('',(0.,0.,1.));
#4649=DIRECTION('',(0.,0.,-1.));
#4650=DIRECTION('',(0.,-1.,0.));
#4651=DIRECTION('',(0.,0.,-1.));
#4652=DIRECTION('',(0.,-1.,0.));
#4653=DIRECTION('center_axis',(0.,1.,0.));
#4654=DIRECTION('ref_axis',(0.,0.,1.));
#4655=DIRECTION('',(0.,0.,1.));
#4656=DIRECTION('center_axis',(0.,1.,0.));
#4657=DIRECTION('ref_axis',(0.,0.,1.));
#4658=DIRECTION('center_axis',(-1.,0.,0.));
#4659=DIRECTION('ref_axis',(0.,0.,1.));
#4660=DIRECTION('center_axis',(-1.,0.,0.));
#4661=DIRECTION('ref_axis',(0.,0.,1.));
#4662=DIRECTION('',(0.,-1.,0.));
#4663=DIRECTION('',(0.,-1.,0.));
#4664=DIRECTION('',(0.,0.,1.));
#4665=DIRECTION('',(0.,-1.,0.));
#4666=DIRECTION('',(0.,0.,1.));
#4667=DIRECTION('center_axis',(-1.,0.,0.));
#4668=DIRECTION('ref_axis',(0.,0.,1.));
#4669=DIRECTION('',(0.,-1.,0.));
#4670=DIRECTION('',(3.86108475418265E-15,0.,1.));
#4671=DIRECTION('',(0.,-1.,0.));
#4672=DIRECTION('',(3.86108475418265E-15,0.,1.));
#4673=DIRECTION('',(0.,0.,1.));
#4674=DIRECTION('center_axis',(1.,0.,0.));
#4675=DIRECTION('ref_axis',(0.,0.,-1.));
#4676=DIRECTION('',(0.,0.,1.));
#4677=DIRECTION('',(0.,1.,0.));
#4678=DIRECTION('center_axis',(1.,0.,0.));
#4679=DIRECTION('ref_axis',(0.,0.,-1.));
#4680=DIRECTION('',(0.,0.,-1.));
#4681=DIRECTION('',(0.,-1.,0.));
#4682=DIRECTION('',(0.,0.,-1.));
#4683=DIRECTION('',(0.,-1.,0.));
#4684=DIRECTION('center_axis',(0.,1.,0.));
#4685=DIRECTION('ref_axis',(0.,0.,1.));
#4686=DIRECTION('center_axis',(0.,1.,0.));
#4687=DIRECTION('ref_axis',(0.,0.,1.));
#4688=DIRECTION('center_axis',(0.,-1.,0.));
#4689=DIRECTION('ref_axis',(0.,0.,-1.));
#4690=DIRECTION('',(0.,0.,1.));
#4691=DIRECTION('',(0.,0.,1.));
#4692=DIRECTION('center_axis',(-1.,1.79068229778251E-16,0.));
#4693=DIRECTION('ref_axis',(0.,0.,1.));
#4694=DIRECTION('',(0.,0.,1.));
#4695=DIRECTION('center_axis',(0.,-1.,0.));
#4696=DIRECTION('ref_axis',(0.,0.,-1.));
#4697=DIRECTION('',(0.,0.,1.));
#4698=DIRECTION('center_axis',(-1.,-8.95341148891256E-17,0.));
#4699=DIRECTION('ref_axis',(0.,0.,1.));
#4700=DIRECTION('center_axis',(-1.,0.,0.));
#4701=DIRECTION('ref_axis',(0.,0.,1.));
#4702=DIRECTION('',(0.,0.,1.));
#4703=DIRECTION('',(0.,0.,1.));
#4704=DIRECTION('center_axis',(0.,1.,0.));
#4705=DIRECTION('ref_axis',(0.,0.,1.));
#4706=DIRECTION('',(0.,0.,1.));
#4707=DIRECTION('center_axis',(-1.,0.,0.));
#4708=DIRECTION('ref_axis',(0.,0.,1.));
#4709=DIRECTION('',(0.,0.,1.));
#4710=DIRECTION('center_axis',(0.,1.,0.));
#4711=DIRECTION('ref_axis',(0.,0.,1.));
#4712=DIRECTION('center_axis',(0.,0.,1.));
#4713=DIRECTION('ref_axis',(1.,0.,0.));
#4714=DIRECTION('',(0.,0.,1.));
#4715=DIRECTION('center_axis',(0.,0.,1.));
#4716=DIRECTION('ref_axis',(1.,0.,0.));
#4717=DIRECTION('',(0.,0.,1.));
#4718=DIRECTION('center_axis',(0.,0.,1.));
#4719=DIRECTION('ref_axis',(1.,0.,0.));
#4720=DIRECTION('',(0.,0.,1.));
#4721=DIRECTION('center_axis',(0.,0.,1.));
#4722=DIRECTION('ref_axis',(1.,0.,0.));
#4723=DIRECTION('',(0.,0.,1.));
#4724=DIRECTION('center_axis',(-1.85037170770859E-16,6.53551686595338E-16,
1.));
#4725=DIRECTION('ref_axis',(1.,0.,1.85037170770859E-16));
#4726=DIRECTION('',(-1.,0.,0.));
#4727=DIRECTION('',(0.,1.,0.));
#4728=DIRECTION('center_axis',(-1.85037170770859E-16,6.53551686595338E-16,
1.));
#4729=DIRECTION('ref_axis',(0.,-1.,6.53551686595338E-16));
#4730=DIRECTION('',(1.,0.,0.));
#4731=DIRECTION('',(0.,-1.,0.));
#4732=DIRECTION('',(1.,0.,0.));
#4733=DIRECTION('',(0.,-1.,0.));
#4734=DIRECTION('center_axis',(4.1086505480261E-32,1.,-2.22044604925031E-16));
#4735=DIRECTION('ref_axis',(0.,2.22044604925031E-16,1.));
#4736=DIRECTION('',(-1.,0.,0.));
#4737=DIRECTION('center_axis',(4.1086505480261E-32,1.,-2.22044604925031E-16));
#4738=DIRECTION('ref_axis',(0.,2.22044604925031E-16,1.));
#4739=DIRECTION('center_axis',(4.1086505480261E-32,1.,-2.22044604925031E-16));
#4740=DIRECTION('ref_axis',(0.,2.22044604925031E-16,1.));
#4741=DIRECTION('center_axis',(1.85037170770859E-16,8.71402248793784E-16,
-1.));
#4742=DIRECTION('ref_axis',(-1.,0.,-1.85037170770859E-16));
#4743=DIRECTION('center_axis',(1.85037170770859E-16,8.71402248793784E-16,
-1.));
#4744=DIRECTION('ref_axis',(0.,1.,8.71402248793784E-16));
#4745=DIRECTION('',(0.,-1.,-1.26882631385732E-15));
#4746=DIRECTION('',(0.,-1.,0.));
#4747=DIRECTION('',(-1.,0.,0.));
#4748=DIRECTION('',(0.,-1.,0.));
#4749=DIRECTION('',(-1.,0.,0.));
#4750=DIRECTION('center_axis',(1.85037170770859E-16,8.71402248793784E-16,
-1.));
#4751=DIRECTION('ref_axis',(-1.,0.,-1.85037170770859E-16));
#4752=DIRECTION('',(-1.,0.,0.));
#4753=DIRECTION('',(0.,1.,0.));
#4754=DIRECTION('center_axis',(1.85037170770859E-16,8.71402248793784E-16,
-1.));
#4755=DIRECTION('ref_axis',(0.,1.,8.71402248793784E-16));
#4756=DIRECTION('',(-1.,0.,0.));
#4757=DIRECTION('',(0.,-1.,0.));
#4758=DIRECTION('',(-1.,0.,0.));
#4759=DIRECTION('',(0.,-1.,0.));
#4760=DIRECTION('center_axis',(4.1086505480261E-32,1.,-2.22044604925031E-16));
#4761=DIRECTION('ref_axis',(0.,2.22044604925031E-16,1.));
#4762=DIRECTION('',(-1.,0.,0.));
#4763=DIRECTION('center_axis',(4.1086505480261E-32,1.,-2.22044604925031E-16));
#4764=DIRECTION('ref_axis',(0.,2.22044604925031E-16,1.));
#4765=DIRECTION('center_axis',(4.1086505480261E-32,1.,-2.22044604925031E-16));
#4766=DIRECTION('ref_axis',(0.,2.22044604925031E-16,1.));
#4767=DIRECTION('center_axis',(-1.85037170770859E-16,6.53551686595338E-16,
1.));
#4768=DIRECTION('ref_axis',(1.,0.,1.85037170770859E-16));
#4769=DIRECTION('center_axis',(-1.85037170770859E-16,6.53551686595338E-16,
1.));
#4770=DIRECTION('ref_axis',(0.,-1.,6.53551686595338E-16));
#4771=DIRECTION('',(0.,-1.,1.26882631385731E-15));
#4772=DIRECTION('',(0.,-1.,0.));
#4773=DIRECTION('',(1.,0.,1.28702825139422E-15));
#4774=DIRECTION('',(0.,-1.,0.));
#4775=DIRECTION('',(1.,0.,0.));
#4776=DIRECTION('center_axis',(0.,0.,1.));
#4777=DIRECTION('ref_axis',(1.,0.,0.));
#4778=DIRECTION('',(-1.,0.,0.));
#4779=DIRECTION('',(0.,-1.,0.));
#4780=DIRECTION('',(-1.,0.,0.));
#4781=DIRECTION('center_axis',(0.,0.,-1.));
#4782=DIRECTION('ref_axis',(-1.,0.,0.));
#4783=DIRECTION('',(0.,-1.,0.));
#4784=DIRECTION('',(1.,0.,0.));
#4785=DIRECTION('center_axis',(1.,0.,0.));
#4786=DIRECTION('ref_axis',(0.,0.,-1.));
#4787=DIRECTION('',(0.,0.,1.));
#4788=DIRECTION('center_axis',(-1.,0.,0.));
#4789=DIRECTION('ref_axis',(0.,0.,1.));
#4790=DIRECTION('',(0.,0.,-1.));
#4791=DIRECTION('',(0.,0.,-1.));
#4792=DIRECTION('center_axis',(0.,-1.,0.));
#4793=DIRECTION('ref_axis',(0.,0.,-1.));
#4794=DIRECTION('',(1.,0.,0.));
#4795=DIRECTION('',(0.,0.,-1.));
#4796=DIRECTION('',(-1.,0.,0.));
#4797=DIRECTION('',(0.,0.,1.));
#4798=DIRECTION('',(1.,0.,0.));
#4799=DIRECTION('',(0.,0.,1.));
#4800=DIRECTION('center_axis',(0.,-1.,0.));
#4801=DIRECTION('ref_axis',(0.,0.,-1.));
#4802=DIRECTION('center_axis',(0.,0.,1.));
#4803=DIRECTION('ref_axis',(1.,0.,0.));
#4804=DIRECTION('',(0.,-1.,0.));
#4805=DIRECTION('',(-1.,0.,0.));
#4806=DIRECTION('center_axis',(0.,0.,-1.));
#4807=DIRECTION('ref_axis',(-1.,0.,0.));
#4808=DIRECTION('',(0.,-1.,0.));
#4809=DIRECTION('',(1.,0.,0.));
#4810=DIRECTION('',(1.,0.,0.));
#4811=DIRECTION('center_axis',(-1.,0.,0.));
#4812=DIRECTION('ref_axis',(0.,0.,1.));
#4813=DIRECTION('',(0.,0.,-1.));
#4814=DIRECTION('',(0.,0.,-1.));
#4815=DIRECTION('center_axis',(1.,0.,0.));
#4816=DIRECTION('ref_axis',(0.,0.,-1.));
#4817=DIRECTION('',(0.,0.,1.));
#4818=DIRECTION('center_axis',(0.,1.,0.));
#4819=DIRECTION('ref_axis',(0.,0.,1.));
#4820=DIRECTION('',(-1.,0.,0.));
#4821=DIRECTION('',(0.,0.,1.));
#4822=DIRECTION('',(-1.,0.,0.));
#4823=DIRECTION('',(0.,0.,1.));
#4824=DIRECTION('',(1.,0.,0.));
#4825=DIRECTION('',(0.,0.,-1.));
#4826=DIRECTION('center_axis',(0.,1.,0.));
#4827=DIRECTION('ref_axis',(0.,0.,1.));
#4828=DIRECTION('center_axis',(-1.,0.,0.));
#4829=DIRECTION('ref_axis',(0.,0.,1.));
#4830=DIRECTION('',(0.,-1.,0.));
#4831=DIRECTION('',(0.,0.,-1.));
#4832=DIRECTION('center_axis',(1.,0.,0.));
#4833=DIRECTION('ref_axis',(0.,0.,-1.));
#4834=DIRECTION('',(0.,-1.,0.));
#4835=DIRECTION('',(0.,0.,1.));
#4836=DIRECTION('',(0.,0.,1.));
#4837=DIRECTION('center_axis',(0.,0.,-1.));
#4838=DIRECTION('ref_axis',(-1.,0.,0.));
#4839=DIRECTION('',(1.,0.,0.));
#4840=DIRECTION('',(1.,0.,0.));
#4841=DIRECTION('center_axis',(0.,0.,1.));
#4842=DIRECTION('ref_axis',(1.,0.,0.));
#4843=DIRECTION('',(-1.,0.,0.));
#4844=DIRECTION('center_axis',(0.,-1.,0.));
#4845=DIRECTION('ref_axis',(0.,0.,-1.));
#4846=DIRECTION('',(0.,0.,-1.));
#4847=DIRECTION('',(-1.,0.,0.));
#4848=DIRECTION('',(0.,0.,-1.));
#4849=DIRECTION('',(-1.,0.,0.));
#4850=DIRECTION('',(0.,0.,1.));
#4851=DIRECTION('',(1.,0.,0.));
#4852=DIRECTION('center_axis',(0.,-1.,0.));
#4853=DIRECTION('ref_axis',(0.,0.,-1.));
#4854=DIRECTION('center_axis',(0.,0.,-1.));
#4855=DIRECTION('ref_axis',(-1.,0.,0.));
#4856=DIRECTION('',(0.,-1.,0.));
#4857=DIRECTION('',(1.,0.,0.));
#4858=DIRECTION('center_axis',(0.,0.,1.));
#4859=DIRECTION('ref_axis',(1.,0.,0.));
#4860=DIRECTION('',(0.,-1.,0.));
#4861=DIRECTION('',(-1.,0.,0.));
#4862=DIRECTION('',(-1.,0.,0.));
#4863=DIRECTION('center_axis',(1.,0.,0.));
#4864=DIRECTION('ref_axis',(0.,0.,-1.));
#4865=DIRECTION('',(0.,0.,1.));
#4866=DIRECTION('',(0.,0.,1.));
#4867=DIRECTION('center_axis',(-1.,0.,0.));
#4868=DIRECTION('ref_axis',(0.,0.,1.));
#4869=DIRECTION('',(0.,0.,-1.));
#4870=DIRECTION('center_axis',(0.,1.,0.));
#4871=DIRECTION('ref_axis',(0.,0.,1.));
#4872=DIRECTION('',(1.,0.,0.));
#4873=DIRECTION('',(0.,0.,-1.));
#4874=DIRECTION('',(1.,0.,0.));
#4875=DIRECTION('',(0.,0.,-1.));
#4876=DIRECTION('',(-1.,0.,0.));
#4877=DIRECTION('',(0.,0.,1.));
#4878=DIRECTION('center_axis',(0.,1.,0.));
#4879=DIRECTION('ref_axis',(0.,0.,1.));
#4880=DIRECTION('center_axis',(0.,0.,1.));
#4881=DIRECTION('ref_axis',(1.,0.,0.));
#4882=DIRECTION('',(-1.,0.,0.));
#4883=DIRECTION('center_axis',(0.,0.,-1.));
#4884=DIRECTION('ref_axis',(-1.,0.,0.));
#4885=DIRECTION('',(1.,0.,0.));
#4886=DIRECTION('',(1.,0.,0.));
#4887=DIRECTION('center_axis',(0.,-1.,0.));
#4888=DIRECTION('ref_axis',(0.,0.,-1.));
#4889=DIRECTION('center_axis',(0.,-1.,0.));
#4890=DIRECTION('ref_axis',(0.,0.,-1.));
#4891=DIRECTION('center_axis',(0.,0.,1.));
#4892=DIRECTION('ref_axis',(1.,0.,0.));
#4893=DIRECTION('',(-1.,0.,0.));
#4894=DIRECTION('',(-1.,0.,0.));
#4895=DIRECTION('center_axis',(0.,0.,-1.));
#4896=DIRECTION('ref_axis',(-1.,0.,0.));
#4897=DIRECTION('',(1.,0.,0.));
#4898=DIRECTION('center_axis',(0.,1.,0.));
#4899=DIRECTION('ref_axis',(0.,0.,1.));
#4900=DIRECTION('center_axis',(0.,1.,0.));
#4901=DIRECTION('ref_axis',(0.,0.,1.));
#4902=DIRECTION('center_axis',(0.,0.,-1.));
#4903=DIRECTION('ref_axis',(-1.,0.,0.));
#4904=DIRECTION('center_axis',(0.,0.,1.));
#4905=DIRECTION('ref_axis',(1.,0.,0.));
#4906=DIRECTION('center_axis',(-0.707106781186548,0.,-0.707106781186548));
#4907=DIRECTION('ref_axis',(0.707106781186548,0.,-0.707106781186548));
#4908=DIRECTION('center_axis',(0.,-1.,0.));
#4909=DIRECTION('ref_axis',(0.,0.,-1.));
#4910=DIRECTION('center_axis',(0.,-1.,0.));
#4911=DIRECTION('ref_axis',(0.,0.,-1.));
#4912=DIRECTION('center_axis',(1.,0.,0.));
#4913=DIRECTION('ref_axis',(0.,0.,-1.));
#4914=DIRECTION('center_axis',(0.707106781186548,0.,-0.707106781186548));
#4915=DIRECTION('ref_axis',(0.707106781186548,0.,0.707106781186548));
#4916=DIRECTION('center_axis',(-1.,0.,0.));
#4917=DIRECTION('ref_axis',(0.,0.,1.));
#4918=DIRECTION('center_axis',(-1.,0.,0.));
#4919=DIRECTION('ref_axis',(0.,0.,1.));
#4920=DIRECTION('center_axis',(0.,0.,-1.));
#4921=DIRECTION('ref_axis',(-1.,0.,0.));
#4922=DIRECTION('center_axis',(-0.707106781186547,0.,-0.707106781186548));
#4923=DIRECTION('ref_axis',(0.707106781186548,0.,-0.707106781186547));
#4924=DIRECTION('center_axis',(-1.,0.,0.));
#4925=DIRECTION('ref_axis',(0.,0.,1.));
#4926=DIRECTION('center_axis',(-0.707106781186548,0.,0.707106781186547));
#4927=DIRECTION('ref_axis',(-0.707106781186547,0.,-0.707106781186548));
#4928=DIRECTION('center_axis',(1.,0.,1.85037170770859E-16));
#4929=DIRECTION('ref_axis',(1.85037170770859E-16,0.,-1.));
#4930=DIRECTION('center_axis',(1.,0.,0.));
#4931=DIRECTION('ref_axis',(0.,0.,-1.));
#4932=DIRECTION('center_axis',(-1.85037170770859E-16,0.,1.));
#4933=DIRECTION('ref_axis',(1.,0.,1.85037170770859E-16));
#4934=DIRECTION('center_axis',(1.85037170770859E-16,8.71402248793784E-16,
-1.));
#4935=DIRECTION('ref_axis',(0.,1.,8.71402248793784E-16));
#4936=DIRECTION('center_axis',(1.85037170770859E-16,8.71402248793784E-16,
-1.));
#4937=DIRECTION('ref_axis',(-1.,0.,0.));
#4938=DIRECTION('center_axis',(0.,-1.,0.));
#4939=DIRECTION('ref_axis',(0.,0.,-1.));
#4940=DIRECTION('center_axis',(-1.61241806720166E-31,1.,8.71402248793784E-16));
#4941=DIRECTION('ref_axis',(0.,-8.71402248793784E-16,1.));
#4942=DIRECTION('center_axis',(-1.,0.,-1.85037170770859E-16));
#4943=DIRECTION('ref_axis',(-1.85037170770859E-16,0.,1.));
#4944=DIRECTION('center_axis',(-1.,0.,0.));
#4945=DIRECTION('ref_axis',(0.,0.,1.));
#4946=DIRECTION('center_axis',(-0.707106781186548,0.,0.707106781186547));
#4947=DIRECTION('ref_axis',(-0.707106781186547,0.,-0.707106781186548));
#4948=DIRECTION('center_axis',(0.,1.,8.71402248793784E-16));
#4949=DIRECTION('ref_axis',(0.,-8.71402248793784E-16,1.));
#4950=DIRECTION('center_axis',(0.,-1.,0.));
#4951=DIRECTION('ref_axis',(0.,0.,-1.));
#4952=DIRECTION('center_axis',(0.,0.,-1.));
#4953=DIRECTION('ref_axis',(-1.,0.,0.));
#4954=DIRECTION('center_axis',(-0.707106781186548,0.,-0.707106781186548));
#4955=DIRECTION('ref_axis',(0.707106781186548,0.,-0.707106781186548));
#4956=DIRECTION('center_axis',(1.85037170770859E-16,8.71402248793784E-16,
-1.));
#4957=DIRECTION('ref_axis',(-1.,0.,0.));
#4958=DIRECTION('center_axis',(1.85037170770859E-16,8.71402248793784E-16,
-1.));
#4959=DIRECTION('ref_axis',(0.,1.,8.71402248793784E-16));
#4960=DIRECTION('center_axis',(-1.,0.,0.));
#4961=DIRECTION('ref_axis',(0.,0.,1.));
#4962=DIRECTION('center_axis',(-0.707106781186548,0.,0.707106781186548));
#4963=DIRECTION('ref_axis',(-0.707106781186548,0.,-0.707106781186548));
#4964=DIRECTION('center_axis',(0.,0.,-1.));
#4965=DIRECTION('ref_axis',(-1.,0.,0.));
#4966=DIRECTION('center_axis',(-0.707106781186548,0.,-0.707106781186548));
#4967=DIRECTION('ref_axis',(0.707106781186548,0.,-0.707106781186548));
#4968=DIRECTION('center_axis',(0.,0.,-1.));
#4969=DIRECTION('ref_axis',(-1.,0.,0.));
#4970=DIRECTION('center_axis',(0.,0.,1.));
#4971=DIRECTION('ref_axis',(1.,0.,0.));
#4972=DIRECTION('center_axis',(1.,0.,0.));
#4973=DIRECTION('ref_axis',(0.,0.,-1.));
#4974=DIRECTION('center_axis',(1.,0.,0.));
#4975=DIRECTION('ref_axis',(0.,0.,-1.));
#4976=DIRECTION('center_axis',(1.,0.,0.));
#4977=DIRECTION('ref_axis',(0.,0.,-1.));
#4978=DIRECTION('center_axis',(0.,-1.,0.));
#4979=DIRECTION('ref_axis',(0.,0.,-1.));
#4980=DIRECTION('center_axis',(0.,1.,0.));
#4981=DIRECTION('ref_axis',(0.,0.,1.));
#4982=DIRECTION('center_axis',(0.,0.,1.));
#4983=DIRECTION('ref_axis',(1.,0.,0.));
#4984=DIRECTION('center_axis',(0.,0.,-1.));
#4985=DIRECTION('ref_axis',(-1.,0.,0.));
#4986=DIRECTION('center_axis',(0.707106781186548,0.,0.707106781186548));
#4987=DIRECTION('ref_axis',(-0.707106781186548,0.,0.707106781186548));
#4988=DIRECTION('center_axis',(0.,-1.,0.));
#4989=DIRECTION('ref_axis',(0.,0.,-1.));
#4990=DIRECTION('center_axis',(0.,-1.,0.));
#4991=DIRECTION('ref_axis',(0.,0.,-1.));
#4992=DIRECTION('center_axis',(-1.,0.,0.));
#4993=DIRECTION('ref_axis',(0.,0.,1.));
#4994=DIRECTION('center_axis',(-0.707106781186548,0.,0.707106781186548));
#4995=DIRECTION('ref_axis',(-0.707106781186548,0.,-0.707106781186548));
#4996=DIRECTION('center_axis',(1.,0.,0.));
#4997=DIRECTION('ref_axis',(0.,0.,-1.));
#4998=DIRECTION('center_axis',(1.,0.,0.));
#4999=DIRECTION('ref_axis',(0.,0.,-1.));
#5000=DIRECTION('center_axis',(0.,0.,1.));
#5001=DIRECTION('ref_axis',(1.,0.,0.));
#5002=DIRECTION('center_axis',(0.707106781186547,0.,0.707106781186548));
#5003=DIRECTION('ref_axis',(-0.707106781186548,0.,0.707106781186547));
#5004=DIRECTION('center_axis',(-1.,0.,0.));
#5005=DIRECTION('ref_axis',(0.,0.,1.));
#5006=DIRECTION('center_axis',(-0.707106781186548,0.,0.707106781186548));
#5007=DIRECTION('ref_axis',(-0.707106781186548,0.,-0.707106781186548));
#5008=DIRECTION('center_axis',(-1.,0.,-1.85037170770859E-16));
#5009=DIRECTION('ref_axis',(-1.85037170770859E-16,0.,1.));
#5010=DIRECTION('center_axis',(-1.,0.,0.));
#5011=DIRECTION('ref_axis',(0.,0.,1.));
#5012=DIRECTION('center_axis',(0.,0.,1.));
#5013=DIRECTION('ref_axis',(1.,0.,0.));
#5014=DIRECTION('center_axis',(-1.85037170770859E-16,6.53551686595338E-16,
1.));
#5015=DIRECTION('ref_axis',(0.,-1.,6.53551686595338E-16));
#5016=DIRECTION('center_axis',(-1.85037170770859E-16,6.53551686595338E-16,
1.));
#5017=DIRECTION('ref_axis',(1.,0.,0.));
#5018=DIRECTION('center_axis',(0.,-1.,0.));
#5019=DIRECTION('ref_axis',(0.,0.,-1.));
#5020=DIRECTION('center_axis',(0.,-1.,6.53551686595338E-16));
#5021=DIRECTION('ref_axis',(0.,-6.53551686595338E-16,-1.));
#5022=DIRECTION('center_axis',(0.,1.,0.));
#5023=DIRECTION('ref_axis',(0.,0.,1.));
#5024=DIRECTION('center_axis',(0.,-1.,0.));
#5025=DIRECTION('ref_axis',(0.,0.,-1.));
#5026=DIRECTION('center_axis',(0.,0.,1.));
#5027=DIRECTION('ref_axis',(1.,0.,0.));
#5028=DIRECTION('center_axis',(0.707106781186548,0.,-0.707106781186548));
#5029=DIRECTION('ref_axis',(0.707106781186548,0.,0.707106781186548));
#5030=DIRECTION('center_axis',(0.,0.,-1.));
#5031=DIRECTION('ref_axis',(-1.,0.,0.));
#5032=DIRECTION('center_axis',(-1.,0.,0.));
#5033=DIRECTION('ref_axis',(0.,0.,1.));
#5034=DIRECTION('center_axis',(-1.,0.,0.));
#5035=DIRECTION('ref_axis',(0.,0.,1.));
#5036=DIRECTION('center_axis',(1.,0.,0.));
#5037=DIRECTION('ref_axis',(0.,0.,-1.));
#5038=DIRECTION('center_axis',(0.707106781186548,0.,0.707106781186548));
#5039=DIRECTION('ref_axis',(0.707106781186548,0.,-0.707106781186548));
#5040=DIRECTION('center_axis',(1.,0.,0.));
#5041=DIRECTION('ref_axis',(0.,0.,-1.));
#5042=DIRECTION('center_axis',(0.707106781186547,0.,0.707106781186548));
#5043=DIRECTION('ref_axis',(0.707106781186548,0.,-0.707106781186547));
#5044=DIRECTION('center_axis',(0.,0.,1.));
#5045=DIRECTION('ref_axis',(1.,0.,0.));
#5046=DIRECTION('center_axis',(0.707106781186548,0.,-0.707106781186547));
#5047=DIRECTION('ref_axis',(0.707106781186547,0.,0.707106781186548));
#5048=DIRECTION('center_axis',(1.85037170770859E-16,0.,-1.));
#5049=DIRECTION('ref_axis',(-1.,0.,-1.85037170770859E-16));
#5050=DIRECTION('center_axis',(-1.85037170770859E-16,6.53551686595338E-16,
1.));
#5051=DIRECTION('ref_axis',(0.,-1.,6.53551686595338E-16));
#5052=DIRECTION('center_axis',(1.,0.,1.85037170770859E-16));
#5053=DIRECTION('ref_axis',(1.85037170770859E-16,0.,-1.));
#5054=DIRECTION('center_axis',(1.,0.,0.));
#5055=DIRECTION('ref_axis',(0.,0.,-1.));
#5056=DIRECTION('center_axis',(-1.85037170770859E-16,6.53551686595338E-16,
1.));
#5057=DIRECTION('ref_axis',(1.,0.,0.));
#5058=DIRECTION('center_axis',(0.,-1.,0.));
#5059=DIRECTION('ref_axis',(0.,0.,-1.));
#5060=DIRECTION('center_axis',(-1.20931355040125E-31,-1.,6.53551686595338E-16));
#5061=DIRECTION('ref_axis',(0.,-6.53551686595338E-16,-1.));
#5062=DIRECTION('center_axis',(0.,-1.,0.));
#5063=DIRECTION('ref_axis',(0.,0.,-1.));
#5064=DIRECTION('',(0.,-1.,0.));
#5065=DIRECTION('center_axis',(0.,-1.,0.));
#5066=DIRECTION('ref_axis',(0.,0.,-1.));
#5067=DIRECTION('',(0.,-1.,0.));
#5068=DIRECTION('axis',(0.,0.,1.));
#5069=DIRECTION('refdir',(1.,0.,0.));
#5070=DIRECTION('center_axis',(1.,1.42336285208353E-16,0.));
#5071=DIRECTION('ref_axis',(0.,0.,-1.));
#5072=DIRECTION('',(9.10952225333462E-17,-1.,0.));
#5073=DIRECTION('',(0.,0.,-1.));
#5074=DIRECTION('',(9.10952225333462E-17,-1.,0.));
#5075=DIRECTION('',(0.,0.,-1.));
#5076=DIRECTION('center_axis',(0.,1.,0.));
#5077=DIRECTION('ref_axis',(0.,0.,1.));
#5078=DIRECTION('',(1.,0.,0.));
#5079=DIRECTION('',(0.,0.,-1.));
#5080=DIRECTION('',(1.,0.,0.));
#5081=DIRECTION('center_axis',(1.,2.84672570416707E-16,0.));
#5082=DIRECTION('ref_axis',(0.,0.,-1.));
#5083=DIRECTION('',(3.64380890133385E-16,-1.,0.));
#5084=DIRECTION('',(0.,0.,-1.));
#5085=DIRECTION('',(3.64380890133385E-16,-1.,0.));
#5086=DIRECTION('center_axis',(0.,1.,0.));
#5087=DIRECTION('ref_axis',(0.,0.,1.));
#5088=DIRECTION('',(1.,0.,0.));
#5089=DIRECTION('',(1.,0.,0.));
#5090=DIRECTION('center_axis',(0.,0.,1.));
#5091=DIRECTION('ref_axis',(1.,0.,0.));
#5092=DIRECTION('center_axis',(0.,0.,1.));
#5093=DIRECTION('ref_axis',(1.,0.,0.));
#5094=DIRECTION('',(-1.,0.,0.));
#5095=DIRECTION('center_axis',(0.,0.,1.));
#5096=DIRECTION('ref_axis',(1.,0.,0.));
#5097=DIRECTION('',(1.,3.28954970259306E-16,0.));
#5098=DIRECTION('center_axis',(0.,0.,1.));
#5099=DIRECTION('ref_axis',(1.,0.,0.));
#5100=DIRECTION('',(-1.,0.,0.));
#5101=DIRECTION('center_axis',(0.,0.,1.));
#5102=DIRECTION('ref_axis',(1.,0.,0.));
#5103=DIRECTION('',(1.,3.28954970259306E-16,0.));
#5104=DIRECTION('center_axis',(0.,0.,1.));
#5105=DIRECTION('ref_axis',(1.,0.,0.));
#5106=DIRECTION('',(-1.,-6.57909940518611E-16,0.));
#5107=DIRECTION('center_axis',(0.,0.,1.));
#5108=DIRECTION('ref_axis',(1.,0.,0.));
#5109=DIRECTION('',(1.,-3.28954970259306E-16,0.));
#5110=DIRECTION('center_axis',(0.,0.,1.));
#5111=DIRECTION('ref_axis',(1.,0.,0.));
#5112=DIRECTION('',(-1.,0.,0.));
#5113=DIRECTION('center_axis',(0.,0.,1.));
#5114=DIRECTION('ref_axis',(1.,0.,0.));
#5115=DIRECTION('',(1.,6.57909940518611E-16,0.));
#5116=DIRECTION('center_axis',(0.,0.,1.));
#5117=DIRECTION('ref_axis',(1.,0.,0.));
#5118=DIRECTION('',(-1.,-6.57909940518611E-16,0.));
#5119=DIRECTION('center_axis',(0.,0.,1.));
#5120=DIRECTION('ref_axis',(1.,0.,0.));
#5121=DIRECTION('',(1.,0.,0.));
#5122=DIRECTION('center_axis',(0.,0.,1.));
#5123=DIRECTION('ref_axis',(1.,0.,0.));
#5124=DIRECTION('center_axis',(0.,0.,1.));
#5125=DIRECTION('ref_axis',(-1.,0.,0.));
#5126=DIRECTION('center_axis',(0.,0.,1.));
#5127=DIRECTION('ref_axis',(-1.,0.,0.));
#5128=DIRECTION('center_axis',(0.,0.,1.));
#5129=DIRECTION('ref_axis',(1.,0.,0.));
#5130=DIRECTION('center_axis',(0.,0.,1.));
#5131=DIRECTION('ref_axis',(1.,0.,0.));
#5132=DIRECTION('',(-1.,0.,0.));
#5133=DIRECTION('center_axis',(0.,0.,1.));
#5134=DIRECTION('ref_axis',(1.,0.,0.));
#5135=DIRECTION('',(1.,3.28954970259306E-16,0.));
#5136=DIRECTION('center_axis',(0.,0.,1.));
#5137=DIRECTION('ref_axis',(1.,0.,0.));
#5138=DIRECTION('',(-1.,0.,0.));
#5139=DIRECTION('center_axis',(0.,0.,1.));
#5140=DIRECTION('ref_axis',(1.,0.,0.));
#5141=DIRECTION('',(1.,3.28954970259306E-16,0.));
#5142=DIRECTION('center_axis',(0.,0.,1.));
#5143=DIRECTION('ref_axis',(1.,0.,0.));
#5144=DIRECTION('',(-1.,-6.57909940518611E-16,0.));
#5145=DIRECTION('center_axis',(0.,0.,1.));
#5146=DIRECTION('ref_axis',(1.,0.,0.));
#5147=DIRECTION('',(1.,-3.28954970259306E-16,0.));
#5148=DIRECTION('center_axis',(0.,0.,1.));
#5149=DIRECTION('ref_axis',(1.,0.,0.));
#5150=DIRECTION('',(-1.,0.,0.));
#5151=DIRECTION('center_axis',(0.,0.,1.));
#5152=DIRECTION('ref_axis',(1.,0.,0.));
#5153=DIRECTION('',(1.,6.57909940518611E-16,0.));
#5154=DIRECTION('center_axis',(0.,0.,1.));
#5155=DIRECTION('ref_axis',(1.,0.,0.));
#5156=DIRECTION('',(-1.,-6.57909940518611E-16,0.));
#5157=DIRECTION('center_axis',(0.,0.,1.));
#5158=DIRECTION('ref_axis',(1.,0.,0.));
#5159=DIRECTION('',(1.,0.,0.));
#5160=DIRECTION('center_axis',(0.,0.,1.));
#5161=DIRECTION('ref_axis',(1.,0.,0.));
#5162=DIRECTION('center_axis',(0.,0.,1.));
#5163=DIRECTION('ref_axis',(1.,0.,0.));
#5164=DIRECTION('center_axis',(0.,0.,1.));
#5165=DIRECTION('ref_axis',(1.,0.,0.));
#5166=DIRECTION('center_axis',(0.,0.,1.));
#5167=DIRECTION('ref_axis',(1.,0.,0.));
#5168=DIRECTION('center_axis',(0.,0.,1.));
#5169=DIRECTION('ref_axis',(1.,0.,0.));
#5170=DIRECTION('center_axis',(0.,0.,1.));
#5171=DIRECTION('ref_axis',(1.,0.,0.));
#5172=DIRECTION('',(0.,0.,1.));
#5173=DIRECTION('center_axis',(0.,0.,1.));
#5174=DIRECTION('ref_axis',(1.,0.,0.));
#5175=DIRECTION('',(0.,0.,1.));
#5176=DIRECTION('center_axis',(0.,0.,1.));
#5177=DIRECTION('ref_axis',(1.,0.,0.));
#5178=DIRECTION('',(0.,0.,1.));
#5179=DIRECTION('center_axis',(0.,0.,1.));
#5180=DIRECTION('ref_axis',(1.,0.,0.));
#5181=DIRECTION('',(0.,0.,1.));
#5182=DIRECTION('center_axis',(0.,0.,1.));
#5183=DIRECTION('ref_axis',(-1.,1.22464679914735E-16,0.));
#5184=DIRECTION('',(0.,0.,1.));
#5185=DIRECTION('',(0.,0.,1.));
#5186=DIRECTION('center_axis',(-7.70988211545248E-16,1.,0.));
#5187=DIRECTION('ref_axis',(0.,0.,1.));
#5188=DIRECTION('',(0.,0.,1.));
#5189=DIRECTION('center_axis',(0.,0.,1.));
#5190=DIRECTION('ref_axis',(1.,0.,0.));
#5191=DIRECTION('',(0.,0.,1.));
#5192=DIRECTION('center_axis',(-2.56996070515083E-16,-1.,0.));
#5193=DIRECTION('ref_axis',(0.,0.,-1.));
#5194=DIRECTION('center_axis',(0.,0.,1.));
#5195=DIRECTION('ref_axis',(-1.,1.22464679914735E-16,0.));
#5196=DIRECTION('',(0.,0.,1.));
#5197=DIRECTION('',(0.,0.,1.));
#5198=DIRECTION('center_axis',(0.,1.,0.));
#5199=DIRECTION('ref_axis',(0.,0.,1.));
#5200=DIRECTION('',(0.,0.,1.));
#5201=DIRECTION('center_axis',(0.,0.,1.));
#5202=DIRECTION('ref_axis',(1.,0.,0.));
#5203=DIRECTION('',(0.,0.,1.));
#5204=DIRECTION('center_axis',(5.13992141030165E-16,-1.,0.));
#5205=DIRECTION('ref_axis',(0.,0.,-1.));
#5206=DIRECTION('center_axis',(0.,0.,1.));
#5207=DIRECTION('ref_axis',(-1.,1.22464679914735E-16,0.));
#5208=DIRECTION('',(0.,0.,1.));
#5209=DIRECTION('',(0.,0.,1.));
#5210=DIRECTION('center_axis',(-7.70988211545248E-16,1.,0.));
#5211=DIRECTION('ref_axis',(0.,0.,1.));
#5212=DIRECTION('',(0.,0.,1.));
#5213=DIRECTION('center_axis',(0.,0.,1.));
#5214=DIRECTION('ref_axis',(1.,0.,0.));
#5215=DIRECTION('',(0.,0.,1.));
#5216=DIRECTION('center_axis',(-2.56996070515083E-16,-1.,0.));
#5217=DIRECTION('ref_axis',(0.,0.,-1.));
#5218=DIRECTION('center_axis',(0.,0.,1.));
#5219=DIRECTION('ref_axis',(-1.,1.22464679914735E-16,0.));
#5220=DIRECTION('',(0.,0.,1.));
#5221=DIRECTION('',(0.,0.,1.));
#5222=DIRECTION('center_axis',(0.,1.,0.));
#5223=DIRECTION('ref_axis',(0.,0.,1.));
#5224=DIRECTION('',(0.,0.,1.));
#5225=DIRECTION('center_axis',(0.,0.,1.));
#5226=DIRECTION('ref_axis',(1.,0.,0.));
#5227=DIRECTION('',(0.,0.,1.));
#5228=DIRECTION('center_axis',(5.13992141030165E-16,-1.,0.));
#5229=DIRECTION('ref_axis',(0.,0.,-1.));
#5230=DIRECTION('center_axis',(0.,0.,1.));
#5231=DIRECTION('ref_axis',(-1.,1.22464679914735E-16,0.));
#5232=DIRECTION('',(0.,0.,1.));
#5233=DIRECTION('',(0.,0.,1.));
#5234=DIRECTION('center_axis',(-2.56996070515083E-16,1.,0.));
#5235=DIRECTION('ref_axis',(0.,0.,1.));
#5236=DIRECTION('',(0.,0.,1.));
#5237=DIRECTION('center_axis',(0.,0.,1.));
#5238=DIRECTION('ref_axis',(1.,0.,0.));
#5239=DIRECTION('',(0.,0.,1.));
#5240=DIRECTION('center_axis',(2.56996070515083E-16,-1.,0.));
#5241=DIRECTION('ref_axis',(0.,0.,-1.));
#5242=DIRECTION('',(0.,0.,1.));
#5243=DIRECTION('',(1.,0.,0.));
#5244=DIRECTION('',(0.,0.,1.));
#5245=DIRECTION('',(1.,0.,0.));
#5246=DIRECTION('',(0.,0.,-1.));
#5247=DIRECTION('',(-1.,0.,0.));
#5248=DIRECTION('axis',(0.,0.,1.));
#5249=DIRECTION('refdir',(1.,0.,0.));
#5250=DIRECTION('center_axis',(0.,-1.,0.));
#5251=DIRECTION('ref_axis',(0.,0.,-1.));
#5252=DIRECTION('center_axis',(0.,-1.,0.));
#5253=DIRECTION('ref_axis',(0.,0.,-1.));
#5254=DIRECTION('',(0.,1.,0.));
#5255=DIRECTION('center_axis',(0.,-1.,0.));
#5256=DIRECTION('ref_axis',(0.,0.,-1.));
#5257=DIRECTION('',(0.,1.,0.));
#5258=DIRECTION('center_axis',(0.,-1.,0.));
#5259=DIRECTION('ref_axis',(0.,0.,-1.));
#5260=DIRECTION('',(0.,1.,0.));
#5261=DIRECTION('center_axis',(0.,-1.,0.));
#5262=DIRECTION('ref_axis',(0.,0.,-1.));
#5263=DIRECTION('',(0.,1.,0.));
#5264=DIRECTION('center_axis',(0.,-1.,0.));
#5265=DIRECTION('ref_axis',(0.,0.,-1.));
#5266=DIRECTION('',(0.,1.,0.));
#5267=DIRECTION('center_axis',(0.,-1.,0.));
#5268=DIRECTION('ref_axis',(0.,0.,-1.));
#5269=DIRECTION('center_axis',(0.,-1.,0.));
#5270=DIRECTION('ref_axis',(0.,0.,-1.));
#5271=DIRECTION('',(2.75077823593892E-16,0.,-1.));
#5272=DIRECTION('',(-1.,0.,0.));
#5273=DIRECTION('',(4.95140082469005E-16,0.,1.));
#5274=DIRECTION('',(-4.95140082469005E-16,0.,1.));
#5275=DIRECTION('',(1.,0.,0.));
#5276=DIRECTION('',(-2.75077823593892E-16,0.,-1.));
#5277=DIRECTION('center_axis',(0.,1.,0.));
#5278=DIRECTION('ref_axis',(0.,0.,1.));
#5279=DIRECTION('center_axis',(0.,-1.,0.));
#5280=DIRECTION('ref_axis',(0.,0.,-1.));
#5281=DIRECTION('center_axis',(0.,-1.,0.));
#5282=DIRECTION('ref_axis',(0.,0.,-1.));
#5283=DIRECTION('',(1.,0.,0.));
#5284=DIRECTION('',(-4.95140082469005E-16,0.,1.));
#5285=DIRECTION('',(-2.75077823593892E-16,0.,-1.));
#5286=DIRECTION('center_axis',(1.,0.,-3.00866369555819E-16));
#5287=DIRECTION('ref_axis',(-3.00866369555819E-16,0.,-1.));
#5288=DIRECTION('',(0.,1.,0.));
#5289=DIRECTION('center_axis',(-1.,0.,-4.72790009302002E-16));
#5290=DIRECTION('ref_axis',(-4.72790009302002E-16,0.,1.));
#5291=DIRECTION('',(0.,1.,0.));
#5292=DIRECTION('center_axis',(0.,0.,1.));
#5293=DIRECTION('ref_axis',(1.,0.,0.));
#5294=DIRECTION('center_axis',(0.,-1.,0.));
#5295=DIRECTION('ref_axis',(0.,0.,-1.));
#5296=DIRECTION('',(4.95140082469005E-16,0.,1.));
#5297=DIRECTION('',(-1.,0.,0.));
#5298=DIRECTION('',(2.75077823593892E-16,0.,-1.));
#5299=DIRECTION('center_axis',(1.,0.,3.00866369555819E-16));
#5300=DIRECTION('ref_axis',(3.00866369555819E-16,0.,-1.));
#5301=DIRECTION('',(0.,1.,0.));
#5302=DIRECTION('center_axis',(0.,0.,-1.));
#5303=DIRECTION('ref_axis',(-1.,0.,0.));
#5304=DIRECTION('',(0.,1.,0.));
#5305=DIRECTION('center_axis',(-1.,0.,4.72790009302002E-16));
#5306=DIRECTION('ref_axis',(4.72790009302002E-16,0.,1.));
#5307=DIRECTION('center_axis',(0.,1.,0.));
#5308=DIRECTION('ref_axis',(0.,0.,1.));
#5309=DIRECTION('center_axis',(0.,1.,0.));
#5310=DIRECTION('ref_axis',(0.,0.,1.));
#5311=DIRECTION('',(-1.0673500138323E-17,0.996194698091745,-0.0871557427476582));
#5312=DIRECTION('center_axis',(0.,1.,0.));
#5313=DIRECTION('ref_axis',(0.,0.,1.));
#5314=DIRECTION('axis',(0.,0.,1.));
#5315=DIRECTION('refdir',(1.,0.,0.));
#5316=DIRECTION('center_axis',(-1.,0.,0.));
#5317=DIRECTION('ref_axis',(0.,0.,1.));
#5318=DIRECTION('center_axis',(-1.,0.,0.));
#5319=DIRECTION('ref_axis',(0.,0.,1.));
#5320=DIRECTION('center_axis',(0.,-1.,1.22464679914735E-16));
#5321=DIRECTION('ref_axis',(0.,-1.22464679914735E-16,-1.));
#5322=DIRECTION('center_axis',(-1.,0.,0.));
#5323=DIRECTION('ref_axis',(0.,0.,1.));
#5324=DIRECTION('center_axis',(-1.,0.,0.));
#5325=DIRECTION('ref_axis',(0.,0.,1.));
#5326=DIRECTION('center_axis',(-1.,0.,0.));
#5327=DIRECTION('ref_axis',(0.,0.,1.));
#5328=DIRECTION('center_axis',(1.,0.,0.));
#5329=DIRECTION('ref_axis',(0.,0.,-1.));
#5330=DIRECTION('center_axis',(1.,0.,0.));
#5331=DIRECTION('ref_axis',(0.,0.,-1.));
#5332=DIRECTION('',(-1.,0.,0.));
#5333=DIRECTION('center_axis',(1.,0.,0.));
#5334=DIRECTION('ref_axis',(0.,0.,-1.));
#5335=DIRECTION('center_axis',(1.,0.,0.));
#5336=DIRECTION('ref_axis',(0.,0.,-1.));
#5337=DIRECTION('center_axis',(1.,0.,0.));
#5338=DIRECTION('ref_axis',(0.,0.,-1.));
#5339=DIRECTION('',(-1.,0.,0.));
#5340=DIRECTION('center_axis',(1.,0.,0.));
#5341=DIRECTION('ref_axis',(0.,0.,-1.));
#5342=DIRECTION('center_axis',(1.,0.,0.));
#5343=DIRECTION('ref_axis',(0.,0.,-1.));
#5344=DIRECTION('center_axis',(1.,0.,0.));
#5345=DIRECTION('ref_axis',(0.,0.,-1.));
#5346=DIRECTION('center_axis',(1.,0.,0.));
#5347=DIRECTION('ref_axis',(0.,0.,-1.));
#5348=DIRECTION('center_axis',(1.,0.,0.));
#5349=DIRECTION('ref_axis',(0.,0.,-1.));
#5350=DIRECTION('center_axis',(0.,-1.,-1.22464679914735E-16));
#5351=DIRECTION('ref_axis',(0.,-1.22464679914735E-16,1.));
#5352=DIRECTION('center_axis',(1.,0.,0.));
#5353=DIRECTION('ref_axis',(0.,0.,-1.));
#5354=DIRECTION('center_axis',(1.,0.,0.));
#5355=DIRECTION('ref_axis',(0.,0.,-1.));
#5356=DIRECTION('',(1.,0.,0.));
#5357=DIRECTION('center_axis',(1.,0.,0.));
#5358=DIRECTION('ref_axis',(0.,0.,-1.));
#5359=DIRECTION('center_axis',(1.,0.,0.));
#5360=DIRECTION('ref_axis',(0.,0.,-1.));
#5361=DIRECTION('center_axis',(0.,-1.,-1.22464679914735E-16));
#5362=DIRECTION('ref_axis',(0.,-1.22464679914735E-16,1.));
#5363=DIRECTION('center_axis',(-1.,0.,0.));
#5364=DIRECTION('ref_axis',(0.,0.,1.));
#5365=DIRECTION('center_axis',(-1.,0.,0.));
#5366=DIRECTION('ref_axis',(0.,0.,1.));
#5367=DIRECTION('center_axis',(0.,-1.,1.22464679914735E-16));
#5368=DIRECTION('ref_axis',(0.,-1.22464679914735E-16,-1.));
#5369=DIRECTION('center_axis',(1.,0.,0.));
#5370=DIRECTION('ref_axis',(0.,0.,-1.));
#5371=DIRECTION('center_axis',(1.,0.,0.));
#5372=DIRECTION('ref_axis',(0.,0.,-1.));
#5373=DIRECTION('center_axis',(1.,0.,0.));
#5374=DIRECTION('ref_axis',(0.,0.,-1.));
#5375=DIRECTION('',(1.,0.,0.));
#5376=DIRECTION('center_axis',(1.,0.,0.));
#5377=DIRECTION('ref_axis',(0.,0.,-1.));
#5378=DIRECTION('center_axis',(1.,0.,0.));
#5379=DIRECTION('ref_axis',(0.,0.,-1.));
#5380=DIRECTION('center_axis',(1.,0.,0.));
#5381=DIRECTION('ref_axis',(0.,0.,-1.));
#5382=DIRECTION('',(1.,0.,0.));
#5383=DIRECTION('center_axis',(1.,0.,0.));
#5384=DIRECTION('ref_axis',(0.,0.,-1.));
#5385=DIRECTION('center_axis',(1.,0.,0.));
#5386=DIRECTION('ref_axis',(0.,0.,-1.));
#5387=DIRECTION('center_axis',(1.,0.,0.));
#5388=DIRECTION('ref_axis',(0.,0.,-1.));
#5389=DIRECTION('center_axis',(0.,-1.,-1.22464679914735E-16));
#5390=DIRECTION('ref_axis',(0.,-1.22464679914735E-16,1.));
#5391=DIRECTION('center_axis',(1.,0.,0.));
#5392=DIRECTION('ref_axis',(0.,0.,-1.));
#5393=DIRECTION('center_axis',(1.,0.,0.));
#5394=DIRECTION('ref_axis',(0.,0.,-1.));
#5395=DIRECTION('',(-1.,0.,0.));
#5396=DIRECTION('center_axis',(1.,0.,0.));
#5397=DIRECTION('ref_axis',(0.,0.,-1.));
#5398=DIRECTION('center_axis',(1.,0.,0.));
#5399=DIRECTION('ref_axis',(0.,0.,-1.));
#5400=DIRECTION('center_axis',(0.,-1.,-1.22464679914735E-16));
#5401=DIRECTION('ref_axis',(0.,-1.22464679914735E-16,1.));
#5402=DIRECTION('center_axis',(1.,0.,0.));
#5403=DIRECTION('ref_axis',(0.,0.,-1.));
#5404=DIRECTION('center_axis',(-1.,0.,0.));
#5405=DIRECTION('ref_axis',(0.,0.,1.));
#5406=DIRECTION('axis',(0.,0.,1.));
#5407=DIRECTION('refdir',(1.,0.,0.));
#5408=DIRECTION('center_axis',(0.,0.,-1.));
#5409=DIRECTION('ref_axis',(-1.,0.,0.));
#5410=DIRECTION('center_axis',(0.,0.,1.));
#5411=DIRECTION('ref_axis',(1.,0.,0.));
#5412=DIRECTION('',(0.,0.,1.));
#5413=DIRECTION('center_axis',(0.,0.,1.));
#5414=DIRECTION('ref_axis',(1.,0.,0.));
#5415=DIRECTION('center_axis',(0.,0.,-1.));
#5416=DIRECTION('ref_axis',(-1.,0.,0.));
#5417=DIRECTION('center_axis',(0.,0.,1.));
#5418=DIRECTION('ref_axis',(1.,0.,0.));
#5419=DIRECTION('center_axis',(0.,0.,1.));
#5420=DIRECTION('ref_axis',(1.,0.,0.));
#5421=DIRECTION('',(0.,0.,1.));
#5422=DIRECTION('center_axis',(0.,0.,1.));
#5423=DIRECTION('ref_axis',(1.,0.,0.));
#5424=DIRECTION('center_axis',(0.,0.,1.));
#5425=DIRECTION('ref_axis',(0.50000000000001,-0.866025403784433,0.));
#5426=DIRECTION('center_axis',(0.,0.,1.));
#5427=DIRECTION('ref_axis',(0.50000000000001,-0.866025403784433,0.));
#5428=DIRECTION('',(0.,0.,1.));
#5429=DIRECTION('center_axis',(0.,0.,1.));
#5430=DIRECTION('ref_axis',(0.50000000000001,-0.866025403784433,0.));
#5431=DIRECTION('center_axis',(0.,0.,1.));
#5432=DIRECTION('ref_axis',(-0.499999999999992,-0.866025403784443,0.));
#5433=DIRECTION('center_axis',(0.,0.,1.));
#5434=DIRECTION('ref_axis',(-0.499999999999992,-0.866025403784443,0.));
#5435=DIRECTION('',(0.,0.,1.));
#5436=DIRECTION('center_axis',(0.,0.,1.));
#5437=DIRECTION('ref_axis',(-0.499999999999992,-0.866025403784443,0.));
#5438=DIRECTION('center_axis',(0.,0.,1.));
#5439=DIRECTION('ref_axis',(-1.,0.,0.));
#5440=DIRECTION('center_axis',(0.,0.,1.));
#5441=DIRECTION('ref_axis',(-1.,0.,0.));
#5442=DIRECTION('',(0.,0.,1.));
#5443=DIRECTION('center_axis',(0.,0.,1.));
#5444=DIRECTION('ref_axis',(-1.,0.,0.));
#5445=DIRECTION('center_axis',(0.,0.,1.));
#5446=DIRECTION('ref_axis',(-0.500000000000004,0.866025403784436,0.));
#5447=DIRECTION('center_axis',(0.,0.,1.));
#5448=DIRECTION('ref_axis',(-0.500000000000004,0.866025403784436,0.));
#5449=DIRECTION('',(0.,0.,1.));
#5450=DIRECTION('center_axis',(0.,0.,1.));
#5451=DIRECTION('ref_axis',(-0.500000000000004,0.866025403784436,0.));
#5452=DIRECTION('center_axis',(0.,0.,1.));
#5453=DIRECTION('ref_axis',(0.499999999999998,0.86602540378444,0.));
#5454=DIRECTION('center_axis',(0.,0.,1.));
#5455=DIRECTION('ref_axis',(0.499999999999998,0.86602540378444,0.));
#5456=DIRECTION('',(0.,0.,1.));
#5457=DIRECTION('center_axis',(0.,0.,1.));
#5458=DIRECTION('ref_axis',(0.499999999999998,0.86602540378444,0.));
#5459=DIRECTION('center_axis',(0.,0.,-1.));
#5460=DIRECTION('ref_axis',(-1.,0.,0.));
#5461=DIRECTION('center_axis',(0.,0.,1.));
#5462=DIRECTION('ref_axis',(1.,0.,0.));
#5463=DIRECTION('',(0.,0.,-1.));
#5464=DIRECTION('center_axis',(0.,0.,1.));
#5465=DIRECTION('ref_axis',(1.,0.,0.));
#5466=DIRECTION('center_axis',(0.,0.,-1.));
#5467=DIRECTION('ref_axis',(-1.,0.,0.));
#5468=DIRECTION('center_axis',(0.,0.,1.));
#5469=DIRECTION('ref_axis',(1.,0.,0.));
#5470=DIRECTION('',(0.,0.,-1.));
#5471=DIRECTION('center_axis',(0.,0.,1.));
#5472=DIRECTION('ref_axis',(1.,0.,0.));
#5473=DIRECTION('center_axis',(0.,0.,1.));
#5474=DIRECTION('ref_axis',(1.,0.,0.));
#5475=DIRECTION('center_axis',(0.,0.,1.));
#5476=DIRECTION('ref_axis',(1.,0.,0.));
#5477=DIRECTION('center_axis',(0.,0.,1.));
#5478=DIRECTION('ref_axis',(1.,0.,0.));
#5479=DIRECTION('center_axis',(0.,0.,1.));
#5480=DIRECTION('ref_axis',(1.,0.,0.));
#5481=DIRECTION('center_axis',(0.,0.,1.));
#5482=DIRECTION('ref_axis',(1.,0.,0.));
#5483=DIRECTION('center_axis',(0.,0.,1.));
#5484=DIRECTION('ref_axis',(1.,0.,0.));
#5485=DIRECTION('center_axis',(0.,0.,1.));
#5486=DIRECTION('ref_axis',(1.,0.,0.));
#5487=DIRECTION('center_axis',(0.,0.,1.));
#5488=DIRECTION('ref_axis',(1.,0.,0.));
#5489=DIRECTION('center_axis',(0.,0.,-1.));
#5490=DIRECTION('ref_axis',(-1.,0.,0.));
#5491=DIRECTION('center_axis',(0.,0.,1.));
#5492=DIRECTION('ref_axis',(1.,0.,0.));
#5493=DIRECTION('',(0.,0.,1.));
#5494=DIRECTION('center_axis',(0.,0.,-1.));
#5495=DIRECTION('ref_axis',(-1.,0.,0.));
#5496=DIRECTION('center_axis',(0.,0.,1.));
#5497=DIRECTION('ref_axis',(1.,0.,0.));
#5498=DIRECTION('',(0.,0.,-1.));
#5499=DIRECTION('center_axis',(0.,0.,1.));
#5500=DIRECTION('ref_axis',(1.,0.,0.));
#5501=DIRECTION('center_axis',(0.,0.,-1.));
#5502=DIRECTION('ref_axis',(-1.,0.,0.));
#5503=DIRECTION('',(0.,0.,1.));
#5504=DIRECTION('center_axis',(0.,0.,1.));
#5505=DIRECTION('ref_axis',(1.,0.,0.));
#5506=DIRECTION('center_axis',(0.,0.,1.));
#5507=DIRECTION('ref_axis',(1.,0.,0.));
#5508=DIRECTION('center_axis',(0.,0.,1.));
#5509=DIRECTION('ref_axis',(1.,0.,0.));
#5510=DIRECTION('center_axis',(0.,0.,1.));
#5511=DIRECTION('ref_axis',(1.,0.,0.));
#5512=DIRECTION('',(0.,0.,1.));
#5513=DIRECTION('center_axis',(0.,0.,-1.));
#5514=DIRECTION('ref_axis',(-1.,0.,0.));
#5515=DIRECTION('',(-0.866025403784436,1.0605752387249E-16,0.500000000000004));
#5516=DIRECTION('center_axis',(0.,0.,1.));
#5517=DIRECTION('ref_axis',(1.,0.,0.));
#5518=DIRECTION('center_axis',(0.,0.,1.));
#5519=DIRECTION('ref_axis',(1.,0.,0.));
#5520=DIRECTION('center_axis',(0.,0.,1.));
#5521=DIRECTION('ref_axis',(1.,0.,0.));
#5522=DIRECTION('',(0.866025403784436,1.0605752387249E-16,-0.500000000000004));
#5523=DIRECTION('center_axis',(0.,0.,1.));
#5524=DIRECTION('ref_axis',(1.,0.,0.));
#5525=DIRECTION('center_axis',(0.,0.,1.));
#5526=DIRECTION('ref_axis',(1.,0.,0.));
#5527=DIRECTION('',(0.,0.,-1.));
#5528=DIRECTION('axis',(0.,0.,1.));
#5529=DIRECTION('refdir',(1.,0.,0.));
#5530=DIRECTION('center_axis',(-0.159999999999998,0.987117014340246,0.));
#5531=DIRECTION('ref_axis',(0.,0.,1.));
#5532=DIRECTION('',(0.987117014340246,0.159999999999998,0.));
#5533=DIRECTION('',(0.,0.,1.));
#5534=DIRECTION('',(0.987117014340246,0.159999999999998,0.));
#5535=DIRECTION('',(0.,0.,1.));
#5536=DIRECTION('center_axis',(0.0807792391722015,-0.498366008702133,-0.863195247837398));
#5537=DIRECTION('ref_axis',(-0.995649789053195,0.,-0.0931745542427157));
#5538=DIRECTION('',(0.987117014340246,0.159999999999998,0.));
#5539=DIRECTION('',(0.,0.866025403784436,-0.500000000000004));
#5540=DIRECTION('',(0.,0.866025403784436,-0.500000000000004));
#5541=DIRECTION('center_axis',(0.159999999999998,-0.987117014340246,0.));
#5542=DIRECTION('ref_axis',(0.,0.,-1.));
#5543=DIRECTION('',(0.987117014340246,0.159999999999998,0.));
#5544=DIRECTION('',(0.,0.,-1.));
#5545=DIRECTION('',(0.,0.,-1.));
#5546=DIRECTION('center_axis',(0.,0.,-1.));
#5547=DIRECTION('ref_axis',(-1.,0.,0.));
#5548=DIRECTION('center_axis',(0.,0.,-1.));
#5549=DIRECTION('ref_axis',(-0.189299873786385,-0.98191932346016,0.));
#5550=DIRECTION('',(0.,0.,1.));
#5551=DIRECTION('center_axis',(0.,0.,-1.));
#5552=DIRECTION('ref_axis',(-0.189299873786385,-0.98191932346016,0.));
#5553=DIRECTION('center_axis',(0.,0.,-1.));
#5554=DIRECTION('ref_axis',(-0.1656970702866,-0.986176698618679,0.));
#5555=DIRECTION('',(-0.273557891496469,-0.821684903110675,-0.500000000000006));
#5556=DIRECTION('center_axis',(0.,0.,-1.));
#5557=DIRECTION('ref_axis',(-1.,0.,0.));
#5558=DIRECTION('center_axis',(0.,0.,-1.));
#5559=DIRECTION('ref_axis',(-0.1656970702866,-0.986176698618679,0.));
#5560=DIRECTION('',(0.,0.,-1.));
#5561=DIRECTION('',(0.,-0.86602540378444,-0.499999999999998));
#5562=DIRECTION('',(0.27355789149647,0.821684903110679,-0.5));
#5563=DIRECTION('center_axis',(-0.160000000000002,-0.987117014340245,0.));
#5564=DIRECTION('ref_axis',(0.,0.,-1.));
#5565=DIRECTION('',(-0.987117014340245,0.160000000000002,0.));
#5566=DIRECTION('',(0.,0.,1.));
#5567=DIRECTION('',(-0.987117014340245,0.160000000000002,0.));
#5568=DIRECTION('center_axis',(0.0807792391722037,0.498366008702132,-0.863195247837398));
#5569=DIRECTION('ref_axis',(-0.995649789053195,0.,-0.0931745542427182));
#5570=DIRECTION('',(-0.987117014340245,0.160000000000002,0.));
#5571=DIRECTION('',(-0.273557891496479,-0.821684903110674,-0.500000000000003));
#5572=DIRECTION('center_axis',(0.160000000000002,0.987117014340245,0.));
#5573=DIRECTION('ref_axis',(0.,0.,1.));
#5574=DIRECTION('',(-0.987117014340245,0.160000000000002,0.));
#5575=DIRECTION('',(0.,0.,-1.));
#5576=DIRECTION('center_axis',(0.0807792391722028,0.498366008702126,0.863195247837401));
#5577=DIRECTION('ref_axis',(0.995649789053195,0.,-0.0931745542427167));
#5578=DIRECTION('',(0.27355789149648,0.821684903110677,-0.499999999999997));
#5579=DIRECTION('center_axis',(0.,0.,-1.));
#5580=DIRECTION('ref_axis',(0.999932136628903,-0.0116499844101919,0.));
#5581=DIRECTION('center_axis',(0.,0.,-1.));
#5582=DIRECTION('ref_axis',(-0.148489244032527,0.988914022757615,0.));
#5583=DIRECTION('center_axis',(0.,0.,-1.));
#5584=DIRECTION('ref_axis',(-0.148489244032527,0.988914022757615,0.));
#5585=DIRECTION('center_axis',(0.,0.,-1.));
#5586=DIRECTION('ref_axis',(-0.157990501106671,0.987440631916706,0.));
#5587=DIRECTION('center_axis',(0.,0.,-1.));
#5588=DIRECTION('ref_axis',(0.999997928592931,-0.00203538936013715,0.));
#5589=DIRECTION('center_axis',(0.,0.,-1.));
#5590=DIRECTION('ref_axis',(-0.157990501106671,0.987440631916706,0.));
#5591=DIRECTION('',(0.,-0.86602540378444,-0.499999999999998));
#5592=DIRECTION('center_axis',(0.0807792391722006,-0.498366008702127,0.863195247837401));
#5593=DIRECTION('ref_axis',(0.995649789053195,0.,-0.0931745542427143));
#5594=DIRECTION('',(0.,0.,1.));
#5595=DIRECTION('',(1.,0.,0.));
#5596=DIRECTION('',(0.698446233568507,-5.53024557692392E-32,0.715662531374926));
#5597=DIRECTION('',(0.715662531374926,-6.12323399573679E-17,-0.698446233568507));
#5598=DIRECTION('',(0.20483597868578,0.,0.978796312741236));
#5599=DIRECTION('',(0.,1.,0.));
#5600=DIRECTION('',(0.291256236959876,0.,0.956645077566373));
#5601=DIRECTION('',(0.,1.,0.));
#5602=DIRECTION('',(3.49433275961766E-17,-1.,-1.17373598748293E-16));
#5603=DIRECTION('',(0.702406793140218,-5.89992488414763E-17,0.711775735011018));
#5604=DIRECTION('',(-3.49433275961648E-17,-1.,1.22103614349289E-33));
#5605=DIRECTION('',(1.,-3.49433275961648E-17,-3.49433275961648E-17));
#5606=CARTESIAN_POINT('',(0.,0.,0.));
#5607=CARTESIAN_POINT('',(0.,0.,0.));
#5608=CARTESIAN_POINT('',(0.,0.,0.));
#5609=CARTESIAN_POINT('Origin',(-800.,-535.,300.));
#5610=CARTESIAN_POINT('',(176.,-505.,300.));
#5611=CARTESIAN_POINT('',(-195.,-505.,300.));
#5612=CARTESIAN_POINT('',(176.,-505.,300.));
#5613=CARTESIAN_POINT('',(176.,-533.,300.));
#5614=CARTESIAN_POINT('',(176.,-533.,300.));
#5615=CARTESIAN_POINT('',(250.,-533.,300.));
#5616=CARTESIAN_POINT('',(176.,-533.,300.));
#5617=CARTESIAN_POINT('',(250.,-285.,300.));
#5618=CARTESIAN_POINT('',(250.,-533.,300.));
#5619=CARTESIAN_POINT('',(-800.,-285.,300.));
#5620=CARTESIAN_POINT('',(-800.,-285.,300.));
#5621=CARTESIAN_POINT('',(-800.,-533.,300.));
#5622=CARTESIAN_POINT('',(-800.,-533.,300.));
#5623=CARTESIAN_POINT('',(-726.,-533.,300.));
#5624=CARTESIAN_POINT('',(-800.,-533.,300.));
#5625=CARTESIAN_POINT('',(-726.,-505.,300.));
#5626=CARTESIAN_POINT('',(-726.,-505.,300.));
#5627=CARTESIAN_POINT('',(-355.,-505.,300.));
#5628=CARTESIAN_POINT('',(-355.,-505.,300.));
#5629=CARTESIAN_POINT('',(-355.,-534.,300.));
#5630=CARTESIAN_POINT('',(-355.,-534.,300.));
#5631=CARTESIAN_POINT('',(-195.,-534.,300.));
#5632=CARTESIAN_POINT('',(-355.,-534.,300.));
#5633=CARTESIAN_POINT('',(-195.,-505.,300.));
#5634=CARTESIAN_POINT('',(208.,-325.693069306929,300.));
#5635=CARTESIAN_POINT('Origin',(210.,-325.693069306929,300.));
#5636=CARTESIAN_POINT('',(-122.,-325.693069306929,300.));
#5637=CARTESIAN_POINT('Origin',(-120.,-325.693069306929,300.));
#5638=CARTESIAN_POINT('',(208.,-490.693069306929,300.));
#5639=CARTESIAN_POINT('Origin',(210.,-490.693069306929,300.));
#5640=CARTESIAN_POINT('',(-122.,-490.693069306929,300.));
#5641=CARTESIAN_POINT('Origin',(-120.,-490.693069306929,300.));
#5642=CARTESIAN_POINT('',(-115.,-330.693069306929,300.));
#5643=CARTESIAN_POINT('',(-115.,-485.693069306929,300.));
#5644=CARTESIAN_POINT('',(-115.,-330.693069306929,300.));
#5645=CARTESIAN_POINT('',(205.,-330.693069306929,300.));
#5646=CARTESIAN_POINT('',(-115.,-330.693069306929,300.));
#5647=CARTESIAN_POINT('',(205.,-485.693069306929,300.));
#5648=CARTESIAN_POINT('',(205.,-330.693069306929,300.));
#5649=CARTESIAN_POINT('',(-115.,-485.693069306929,300.));
#5650=CARTESIAN_POINT('',(-435.,-330.693069306929,300.));
#5651=CARTESIAN_POINT('',(-755.,-330.693069306929,300.));
#5652=CARTESIAN_POINT('',(-435.,-330.693069306929,300.));
#5653=CARTESIAN_POINT('',(-435.,-485.693069306929,300.));
#5654=CARTESIAN_POINT('',(-435.,-330.693069306929,300.));
#5655=CARTESIAN_POINT('',(-755.,-485.693069306929,300.));
#5656=CARTESIAN_POINT('',(-435.,-485.693069306929,300.));
#5657=CARTESIAN_POINT('',(-755.,-330.693069306929,300.));
#5658=CARTESIAN_POINT('Origin',(-800.,-535.,300.));
#5659=CARTESIAN_POINT('',(-800.,-533.,-251.));
#5660=CARTESIAN_POINT('',(-800.,-505.,-251.));
#5661=CARTESIAN_POINT('',(-800.,-533.,-251.));
#5662=CARTESIAN_POINT('',(-800.,-505.,251.));
#5663=CARTESIAN_POINT('',(-800.,-505.,-251.));
#5664=CARTESIAN_POINT('',(-800.,-533.,251.));
#5665=CARTESIAN_POINT('',(-800.,-505.,251.));
#5666=CARTESIAN_POINT('',(-800.,-533.,251.));
#5667=CARTESIAN_POINT('',(-800.,-285.,-300.));
#5668=CARTESIAN_POINT('',(-800.,-285.,300.));
#5669=CARTESIAN_POINT('',(-800.,-533.,-300.));
#5670=CARTESIAN_POINT('',(-800.,-533.,-300.));
#5671=CARTESIAN_POINT('',(-800.,-533.,-300.));
#5672=CARTESIAN_POINT('Origin',(-800.,-535.,-300.));
#5673=CARTESIAN_POINT('',(-355.,-505.,-300.));
#5674=CARTESIAN_POINT('',(-726.,-505.,-300.));
#5675=CARTESIAN_POINT('',(-355.,-505.,-300.));
#5676=CARTESIAN_POINT('',(-726.,-533.,-300.));
#5677=CARTESIAN_POINT('',(-726.,-505.,-300.));
#5678=CARTESIAN_POINT('',(-726.,-533.,-300.));
#5679=CARTESIAN_POINT('',(250.,-285.,-300.));
#5680=CARTESIAN_POINT('',(-800.,-285.,-300.));
#5681=CARTESIAN_POINT('',(250.,-533.,-300.));
#5682=CARTESIAN_POINT('',(250.,-533.,-300.));
#5683=CARTESIAN_POINT('',(176.,-533.,-300.));
#5684=CARTESIAN_POINT('',(250.,-533.,-300.));
#5685=CARTESIAN_POINT('',(176.,-505.,-300.));
#5686=CARTESIAN_POINT('',(176.,-533.,-300.));
#5687=CARTESIAN_POINT('',(-195.,-505.,-300.));
#5688=CARTESIAN_POINT('',(176.,-505.,-300.));
#5689=CARTESIAN_POINT('',(-195.,-534.,-300.));
#5690=CARTESIAN_POINT('',(-195.,-505.,-300.));
#5691=CARTESIAN_POINT('',(-355.,-534.,-300.));
#5692=CARTESIAN_POINT('',(-195.,-534.,-300.));
#5693=CARTESIAN_POINT('',(-355.,-534.,-300.));
#5694=CARTESIAN_POINT('Origin',(250.,-535.,300.));
#5695=CARTESIAN_POINT('',(250.,-505.,251.));
#5696=CARTESIAN_POINT('',(250.,-505.,-251.));
#5697=CARTESIAN_POINT('',(250.,-505.,251.));
#5698=CARTESIAN_POINT('',(250.,-533.,-251.));
#5699=CARTESIAN_POINT('',(250.,-505.,-251.));
#5700=CARTESIAN_POINT('',(250.,-533.,-251.));
#5701=CARTESIAN_POINT('',(250.,-285.,300.));
#5702=CARTESIAN_POINT('',(250.,-533.,251.));
#5703=CARTESIAN_POINT('',(250.,-533.,300.));
#5704=CARTESIAN_POINT('',(250.,-533.,251.));
#5705=CARTESIAN_POINT('Origin',(0.,-535.,0.));
#5706=CARTESIAN_POINT('',(-800.,-535.,-250.));
#5707=CARTESIAN_POINT('',(-797.,-535.,-250.));
#5708=CARTESIAN_POINT('',(-800.,-535.,-250.));
#5709=CARTESIAN_POINT('',(-800.,-535.,-300.));
#5710=CARTESIAN_POINT('',(-800.,-535.,-250.));
#5711=CARTESIAN_POINT('',(-725.,-535.,-300.));
#5712=CARTESIAN_POINT('',(-800.,-535.,-300.));
#5713=CARTESIAN_POINT('',(-725.,-535.,-297.));
#5714=CARTESIAN_POINT('',(-725.,-535.,-297.));
#5715=CARTESIAN_POINT('',(-797.,-535.,-297.));
#5716=CARTESIAN_POINT('',(-797.,-535.,-297.));
#5717=CARTESIAN_POINT('',(-797.,-535.,-250.));
#5718=CARTESIAN_POINT('Origin',(0.,-535.,0.));
#5719=CARTESIAN_POINT('',(247.,-535.,-250.));
#5720=CARTESIAN_POINT('',(250.,-535.,-250.));
#5721=CARTESIAN_POINT('',(247.,-535.,-250.));
#5722=CARTESIAN_POINT('',(247.,-535.,-297.));
#5723=CARTESIAN_POINT('',(247.,-535.,-250.));
#5724=CARTESIAN_POINT('',(175.,-535.,-297.));
#5725=CARTESIAN_POINT('',(175.,-535.,-297.));
#5726=CARTESIAN_POINT('',(175.,-535.,-300.));
#5727=CARTESIAN_POINT('',(175.,-535.,-300.));
#5728=CARTESIAN_POINT('',(250.,-535.,-300.));
#5729=CARTESIAN_POINT('',(175.,-535.,-300.));
#5730=CARTESIAN_POINT('',(250.,-535.,-250.));
#5731=CARTESIAN_POINT('Origin',(-800.,-535.,297.));
#5732=CARTESIAN_POINT('',(175.,-505.,297.));
#5733=CARTESIAN_POINT('',(-195.,-505.,297.));
#5734=CARTESIAN_POINT('',(175.,-505.,297.));
#5735=CARTESIAN_POINT('',(-195.,-535.,297.));
#5736=CARTESIAN_POINT('',(-195.,-505.,297.));
#5737=CARTESIAN_POINT('',(-355.,-535.,297.));
#5738=CARTESIAN_POINT('',(-355.,-535.,297.));
#5739=CARTESIAN_POINT('',(-355.,-505.,297.));
#5740=CARTESIAN_POINT('',(-355.,-535.,297.));
#5741=CARTESIAN_POINT('',(-725.,-505.,297.));
#5742=CARTESIAN_POINT('',(-355.,-505.,297.));
#5743=CARTESIAN_POINT('',(-725.,-535.,297.));
#5744=CARTESIAN_POINT('',(-725.,-505.,297.));
#5745=CARTESIAN_POINT('',(-797.,-535.,297.));
#5746=CARTESIAN_POINT('',(-797.,-535.,297.));
#5747=CARTESIAN_POINT('',(-797.,-288.,297.));
#5748=CARTESIAN_POINT('',(-797.,-535.,297.));
#5749=CARTESIAN_POINT('',(247.,-288.,297.));
#5750=CARTESIAN_POINT('',(-797.,-288.,297.));
#5751=CARTESIAN_POINT('',(247.,-535.,297.));
#5752=CARTESIAN_POINT('',(247.,-535.,297.));
#5753=CARTESIAN_POINT('',(175.,-535.,297.));
#5754=CARTESIAN_POINT('',(175.,-535.,297.));
#5755=CARTESIAN_POINT('',(175.,-535.,297.));
#5756=CARTESIAN_POINT('',(-435.,-330.693069306929,297.));
#5757=CARTESIAN_POINT('',(-435.,-485.693069306929,297.));
#5758=CARTESIAN_POINT('',(-435.,-330.693069306929,297.));
#5759=CARTESIAN_POINT('',(-755.,-330.693069306929,297.));
#5760=CARTESIAN_POINT('',(-435.,-330.693069306929,297.));
#5761=CARTESIAN_POINT('',(-755.,-485.693069306929,297.));
#5762=CARTESIAN_POINT('',(-755.,-330.693069306929,297.));
#5763=CARTESIAN_POINT('',(-435.,-485.693069306929,297.));
#5764=CARTESIAN_POINT('',(208.,-325.693069306929,297.));
#5765=CARTESIAN_POINT('Origin',(210.,-325.693069306929,297.));
#5766=CARTESIAN_POINT('',(-122.,-325.693069306929,297.));
#5767=CARTESIAN_POINT('Origin',(-120.,-325.693069306929,297.));
#5768=CARTESIAN_POINT('',(208.,-490.693069306929,297.));
#5769=CARTESIAN_POINT('Origin',(210.,-490.693069306929,297.));
#5770=CARTESIAN_POINT('',(-122.,-490.693069306929,297.));
#5771=CARTESIAN_POINT('Origin',(-120.,-490.693069306929,297.));
#5772=CARTESIAN_POINT('',(-115.,-330.693069306929,297.));
#5773=CARTESIAN_POINT('',(205.,-330.693069306929,297.));
#5774=CARTESIAN_POINT('',(-115.,-330.693069306929,297.));
#5775=CARTESIAN_POINT('',(-115.,-485.693069306929,297.));
#5776=CARTESIAN_POINT('',(-115.,-330.693069306929,297.));
#5777=CARTESIAN_POINT('',(205.,-485.693069306929,297.));
#5778=CARTESIAN_POINT('',(-115.,-485.693069306929,297.));
#5779=CARTESIAN_POINT('',(205.,-330.693069306929,297.));
#5780=CARTESIAN_POINT('Origin',(0.,-535.,0.));
#5781=CARTESIAN_POINT('',(-195.,-535.,-297.));
#5782=CARTESIAN_POINT('',(-195.,-535.,-300.));
#5783=CARTESIAN_POINT('',(-195.,-535.,-297.));
#5784=CARTESIAN_POINT('',(-355.,-535.,-297.));
#5785=CARTESIAN_POINT('',(-355.,-535.,-297.));
#5786=CARTESIAN_POINT('',(-355.,-535.,-300.));
#5787=CARTESIAN_POINT('',(-355.,-535.,-300.));
#5788=CARTESIAN_POINT('',(-355.,-535.,-300.));
#5789=CARTESIAN_POINT('Origin',(0.,-535.,0.));
#5790=CARTESIAN_POINT('',(-195.,-535.,300.));
#5791=CARTESIAN_POINT('',(-195.,-535.,300.));
#5792=CARTESIAN_POINT('',(-355.,-535.,300.));
#5793=CARTESIAN_POINT('',(-355.,-535.,300.));
#5794=CARTESIAN_POINT('',(-355.,-535.,297.));
#5795=CARTESIAN_POINT('Origin',(0.,-535.,0.));
#5796=CARTESIAN_POINT('',(-797.,-535.,250.));
#5797=CARTESIAN_POINT('',(-800.,-535.,250.));
#5798=CARTESIAN_POINT('',(-797.,-535.,250.));
#5799=CARTESIAN_POINT('',(-797.,-535.,297.));
#5800=CARTESIAN_POINT('',(-725.,-535.,300.));
#5801=CARTESIAN_POINT('',(-725.,-535.,300.));
#5802=CARTESIAN_POINT('',(-800.,-535.,300.));
#5803=CARTESIAN_POINT('',(-800.,-535.,300.));
#5804=CARTESIAN_POINT('',(-800.,-535.,300.));
#5805=CARTESIAN_POINT('Origin',(0.,-535.,0.));
#5806=CARTESIAN_POINT('',(250.,-535.,250.));
#5807=CARTESIAN_POINT('',(247.,-535.,250.));
#5808=CARTESIAN_POINT('',(250.,-535.,250.));
#5809=CARTESIAN_POINT('',(250.,-535.,300.));
#5810=CARTESIAN_POINT('',(250.,-535.,300.));
#5811=CARTESIAN_POINT('',(175.,-535.,300.));
#5812=CARTESIAN_POINT('',(175.,-535.,300.));
#5813=CARTESIAN_POINT('',(175.,-535.,297.));
#5814=CARTESIAN_POINT('',(247.,-535.,297.));
#5815=CARTESIAN_POINT('Origin',(0.,-285.,0.));
#5816=CARTESIAN_POINT('',(-500.,-285.,35.));
#5817=CARTESIAN_POINT('Origin',(-500.,-285.,-6.12323399573677E-14));
#5818=CARTESIAN_POINT('',(-4.28626379701574E-15,-285.,35.));
#5819=CARTESIAN_POINT('Origin',(0.,-285.,0.));
#5820=CARTESIAN_POINT('Origin',(-797.,-535.,300.));
#5821=CARTESIAN_POINT('',(-797.,-505.,-250.));
#5822=CARTESIAN_POINT('',(-797.,-535.,-250.));
#5823=CARTESIAN_POINT('',(-797.,-288.,-297.));
#5824=CARTESIAN_POINT('',(-797.,-535.,-297.));
#5825=CARTESIAN_POINT('',(-797.,-288.,297.));
#5826=CARTESIAN_POINT('',(-797.,-505.,250.));
#5827=CARTESIAN_POINT('',(-797.,-505.,250.));
#5828=CARTESIAN_POINT('',(-797.,-505.,-250.));
#5829=CARTESIAN_POINT('Origin',(-800.,-535.,-297.));
#5830=CARTESIAN_POINT('',(-195.,-505.,-297.));
#5831=CARTESIAN_POINT('',(-195.,-505.,-297.));
#5832=CARTESIAN_POINT('',(175.,-505.,-297.));
#5833=CARTESIAN_POINT('',(175.,-505.,-297.));
#5834=CARTESIAN_POINT('',(175.,-535.,-297.));
#5835=CARTESIAN_POINT('',(247.,-288.,-297.));
#5836=CARTESIAN_POINT('',(247.,-535.,-297.));
#5837=CARTESIAN_POINT('',(-797.,-288.,-297.));
#5838=CARTESIAN_POINT('',(-725.,-505.,-297.));
#5839=CARTESIAN_POINT('',(-725.,-505.,-297.));
#5840=CARTESIAN_POINT('',(-355.,-505.,-297.));
#5841=CARTESIAN_POINT('',(-355.,-505.,-297.));
#5842=CARTESIAN_POINT('',(-355.,-535.,-297.));
#5843=CARTESIAN_POINT('Origin',(247.,-535.,300.));
#5844=CARTESIAN_POINT('',(247.,-505.,-250.));
#5845=CARTESIAN_POINT('',(247.,-535.,-250.));
#5846=CARTESIAN_POINT('',(247.,-505.,250.));
#5847=CARTESIAN_POINT('',(247.,-505.,-250.));
#5848=CARTESIAN_POINT('',(247.,-505.,250.));
#5849=CARTESIAN_POINT('',(247.,-288.,297.));
#5850=CARTESIAN_POINT('Origin',(0.,-288.,0.));
#5851=CARTESIAN_POINT('',(-500.,-288.,35.));
#5852=CARTESIAN_POINT('Origin',(-500.,-288.,-6.12323399573677E-14));
#5853=CARTESIAN_POINT('',(-4.28626379701574E-15,-288.,35.));
#5854=CARTESIAN_POINT('Origin',(0.,-288.,0.));
#5855=CARTESIAN_POINT('Origin',(-355.,-535.,-300.));
#5856=CARTESIAN_POINT('',(-355.,-537.,300.));
#5857=CARTESIAN_POINT('',(-355.,-535.,300.));
#5858=CARTESIAN_POINT('',(-355.,-537.,327.60400694353));
#5859=CARTESIAN_POINT('',(-355.,-537.,327.60400694353));
#5860=CARTESIAN_POINT('',(-355.,-534.,327.60400694353));
#5861=CARTESIAN_POINT('',(-355.,-534.,327.60400694353));
#5862=CARTESIAN_POINT('',(-355.,-534.,327.60400694353));
#5863=CARTESIAN_POINT('',(-355.,-505.,297.));
#5864=CARTESIAN_POINT('Origin',(-355.,-505.,-300.));
#5865=CARTESIAN_POINT('',(-725.,-505.,299.));
#5866=CARTESIAN_POINT('Origin',(-726.,-505.,299.));
#5867=CARTESIAN_POINT('',(-725.,-505.,297.));
#5868=CARTESIAN_POINT('Origin',(-725.,-505.,-300.));
#5869=CARTESIAN_POINT('',(-725.,-533.,299.));
#5870=CARTESIAN_POINT('',(-725.,-505.,299.));
#5871=CARTESIAN_POINT('',(-725.,-535.,301.));
#5872=CARTESIAN_POINT('Origin',(-725.,-533.,301.));
#5873=CARTESIAN_POINT('',(-725.,-535.,327.60400694353));
#5874=CARTESIAN_POINT('',(-725.,-535.,301.));
#5875=CARTESIAN_POINT('',(-725.,-537.,327.60400694353));
#5876=CARTESIAN_POINT('',(-725.,-535.,327.60400694353));
#5877=CARTESIAN_POINT('',(-725.,-537.,300.));
#5878=CARTESIAN_POINT('',(-725.,-537.,300.));
#5879=CARTESIAN_POINT('',(-725.,-535.,300.));
#5880=CARTESIAN_POINT('Origin',(175.,-505.,-300.));
#5881=CARTESIAN_POINT('',(175.,-533.,299.));
#5882=CARTESIAN_POINT('',(175.,-535.,301.));
#5883=CARTESIAN_POINT('Origin',(175.,-533.,301.));
#5884=CARTESIAN_POINT('',(175.,-505.,299.));
#5885=CARTESIAN_POINT('',(175.,-533.,299.));
#5886=CARTESIAN_POINT('',(175.,-505.,297.));
#5887=CARTESIAN_POINT('',(175.,-537.,300.));
#5888=CARTESIAN_POINT('',(175.,-535.,300.));
#5889=CARTESIAN_POINT('',(175.,-537.,327.60400694353));
#5890=CARTESIAN_POINT('',(175.,-537.,327.60400694353));
#5891=CARTESIAN_POINT('',(175.,-535.,327.60400694353));
#5892=CARTESIAN_POINT('',(175.,-535.,327.60400694353));
#5893=CARTESIAN_POINT('',(175.,-535.,327.60400694353));
#5894=CARTESIAN_POINT('Origin',(-195.,-505.,-300.));
#5895=CARTESIAN_POINT('',(-195.,-505.,297.));
#5896=CARTESIAN_POINT('Origin',(176.,-505.,299.));
#5897=CARTESIAN_POINT('Origin',(-195.,-535.,-300.));
#5898=CARTESIAN_POINT('',(-195.,-534.,327.60400694353));
#5899=CARTESIAN_POINT('',(-195.,-534.,300.));
#5900=CARTESIAN_POINT('',(-195.,-537.,327.60400694353));
#5901=CARTESIAN_POINT('',(-195.,-534.,327.60400694353));
#5902=CARTESIAN_POINT('',(-195.,-537.,300.));
#5903=CARTESIAN_POINT('',(-195.,-537.,300.));
#5904=CARTESIAN_POINT('',(-195.,-535.,300.));
#5905=CARTESIAN_POINT('Origin',(-355.,-535.,-300.));
#5906=CARTESIAN_POINT('',(-355.,-505.,-300.));
#5907=CARTESIAN_POINT('',(-355.,-534.,-327.60400694353));
#5908=CARTESIAN_POINT('',(-355.,-534.,-300.));
#5909=CARTESIAN_POINT('',(-355.,-537.,-327.60400694353));
#5910=CARTESIAN_POINT('',(-355.,-534.,-327.60400694353));
#5911=CARTESIAN_POINT('',(-355.,-537.,-300.));
#5912=CARTESIAN_POINT('',(-355.,-537.,-300.));
#5913=CARTESIAN_POINT('',(-355.,-535.,-300.));
#5914=CARTESIAN_POINT('Origin',(-355.,-505.,-300.));
#5915=CARTESIAN_POINT('',(-725.,-505.,-299.));
#5916=CARTESIAN_POINT('',(-725.,-505.,-299.));
#5917=CARTESIAN_POINT('Origin',(-726.,-505.,-299.));
#5918=CARTESIAN_POINT('Origin',(-725.,-505.,-300.));
#5919=CARTESIAN_POINT('',(-725.,-533.,-299.));
#5920=CARTESIAN_POINT('',(-725.,-535.,-301.));
#5921=CARTESIAN_POINT('Origin',(-725.,-533.,-301.));
#5922=CARTESIAN_POINT('',(-725.,-505.,-299.));
#5923=CARTESIAN_POINT('',(-725.,-537.,-300.));
#5924=CARTESIAN_POINT('',(-725.,-535.,-300.));
#5925=CARTESIAN_POINT('',(-725.,-537.,-327.60400694353));
#5926=CARTESIAN_POINT('',(-725.,-537.,-327.60400694353));
#5927=CARTESIAN_POINT('',(-725.,-535.,-327.60400694353));
#5928=CARTESIAN_POINT('',(-725.,-535.,-327.60400694353));
#5929=CARTESIAN_POINT('',(-725.,-535.,-327.60400694353));
#5930=CARTESIAN_POINT('Origin',(-195.,-535.,-300.));
#5931=CARTESIAN_POINT('',(-195.,-537.,-300.));
#5932=CARTESIAN_POINT('',(-195.,-535.,-300.));
#5933=CARTESIAN_POINT('',(-195.,-537.,-327.60400694353));
#5934=CARTESIAN_POINT('',(-195.,-537.,-327.60400694353));
#5935=CARTESIAN_POINT('',(-195.,-534.,-327.60400694353));
#5936=CARTESIAN_POINT('',(-195.,-534.,-327.60400694353));
#5937=CARTESIAN_POINT('',(-195.,-534.,-327.60400694353));
#5938=CARTESIAN_POINT('',(-195.,-505.,-300.));
#5939=CARTESIAN_POINT('Origin',(175.,-505.,-300.));
#5940=CARTESIAN_POINT('',(175.,-505.,-299.));
#5941=CARTESIAN_POINT('',(175.,-505.,-299.));
#5942=CARTESIAN_POINT('',(175.,-533.,-299.));
#5943=CARTESIAN_POINT('',(175.,-533.,-299.));
#5944=CARTESIAN_POINT('',(175.,-535.,-301.));
#5945=CARTESIAN_POINT('Origin',(175.,-533.,-301.));
#5946=CARTESIAN_POINT('',(175.,-535.,-327.60400694353));
#5947=CARTESIAN_POINT('',(175.,-535.,-301.));
#5948=CARTESIAN_POINT('',(175.,-537.,-327.60400694353));
#5949=CARTESIAN_POINT('',(175.,-535.,-327.60400694353));
#5950=CARTESIAN_POINT('',(175.,-537.,-300.));
#5951=CARTESIAN_POINT('',(175.,-537.,-300.));
#5952=CARTESIAN_POINT('',(175.,-535.,-300.));
#5953=CARTESIAN_POINT('Origin',(-195.,-505.,-300.));
#5954=CARTESIAN_POINT('Origin',(176.,-505.,-299.));
#5955=CARTESIAN_POINT('Origin',(0.,-330.693069306929,100.));
#5956=CARTESIAN_POINT('',(205.,-330.693069306929,297.));
#5957=CARTESIAN_POINT('',(-115.,-330.693069306929,297.));
#5958=CARTESIAN_POINT('Origin',(205.,-3.67089871045415E-14,100.));
#5959=CARTESIAN_POINT('',(205.,-485.693069306929,297.));
#5960=CARTESIAN_POINT('Origin',(0.,-485.693069306929,100.));
#5961=CARTESIAN_POINT('',(-115.,-485.693069306929,297.));
#5962=CARTESIAN_POINT('Origin',(-115.,-1.02964232122494E-14,100.));
#5963=CARTESIAN_POINT('Origin',(-435.,0.,100.));
#5964=CARTESIAN_POINT('',(-435.,-485.693069306929,297.));
#5965=CARTESIAN_POINT('',(-435.,-330.693069306929,297.));
#5966=CARTESIAN_POINT('Origin',(0.,-485.693069306929,100.));
#5967=CARTESIAN_POINT('',(-755.,-485.693069306929,297.));
#5968=CARTESIAN_POINT('Origin',(-755.,0.,100.));
#5969=CARTESIAN_POINT('',(-755.,-330.693069306929,297.));
#5970=CARTESIAN_POINT('Origin',(0.,-330.693069306929,100.));
#5971=CARTESIAN_POINT('Origin',(-120.,-490.693069306929,280.));
#5972=CARTESIAN_POINT('',(-122.,-490.693069306929,280.));
#5973=CARTESIAN_POINT('Origin',(210.,-490.693069306929,280.));
#5974=CARTESIAN_POINT('',(208.,-490.693069306929,280.));
#5975=CARTESIAN_POINT('Origin',(-120.,-325.693069306929,280.));
#5976=CARTESIAN_POINT('',(-122.,-325.693069306929,280.));
#5977=CARTESIAN_POINT('Origin',(210.,-325.693069306929,280.));
#5978=CARTESIAN_POINT('',(208.,-325.693069306929,280.));
#5979=CARTESIAN_POINT('Origin',(250.,-505.,250.));
#5980=CARTESIAN_POINT('',(249.,-505.,250.));
#5981=CARTESIAN_POINT('',(249.,-505.,250.));
#5982=CARTESIAN_POINT('',(249.,-533.,250.));
#5983=CARTESIAN_POINT('',(249.,-533.,250.));
#5984=CARTESIAN_POINT('',(251.,-535.,250.));
#5985=CARTESIAN_POINT('Origin',(251.,-533.,250.));
#5986=CARTESIAN_POINT('',(277.60400694353,-535.,250.));
#5987=CARTESIAN_POINT('',(251.,-535.,250.));
#5988=CARTESIAN_POINT('',(277.60400694353,-537.,250.));
#5989=CARTESIAN_POINT('',(277.60400694353,-535.,250.));
#5990=CARTESIAN_POINT('',(250.,-537.,250.));
#5991=CARTESIAN_POINT('',(250.,-537.,250.));
#5992=CARTESIAN_POINT('',(250.,-535.,250.));
#5993=CARTESIAN_POINT('Origin',(250.,-505.,-250.));
#5994=CARTESIAN_POINT('',(249.,-505.,-250.));
#5995=CARTESIAN_POINT('',(249.,-505.,-250.));
#5996=CARTESIAN_POINT('Origin',(249.,-505.,-251.));
#5997=CARTESIAN_POINT('Origin',(249.,-505.,251.));
#5998=CARTESIAN_POINT('Origin',(250.,-505.,-250.));
#5999=CARTESIAN_POINT('',(249.,-533.,-250.));
#6000=CARTESIAN_POINT('',(251.,-535.,-250.));
#6001=CARTESIAN_POINT('Origin',(251.,-533.,-250.));
#6002=CARTESIAN_POINT('',(249.,-505.,-250.));
#6003=CARTESIAN_POINT('',(250.,-537.,-250.));
#6004=CARTESIAN_POINT('',(250.,-535.,-250.));
#6005=CARTESIAN_POINT('',(277.60400694353,-537.,-250.));
#6006=CARTESIAN_POINT('',(277.60400694353,-537.,-250.));
#6007=CARTESIAN_POINT('',(277.60400694353,-535.,-250.));
#6008=CARTESIAN_POINT('',(277.60400694353,-535.,-250.));
#6009=CARTESIAN_POINT('',(277.60400694353,-535.,-250.));
#6010=CARTESIAN_POINT('Origin',(250.,-505.,-250.));
#6011=CARTESIAN_POINT('',(-799.,-505.,-250.));
#6012=CARTESIAN_POINT('',(-797.,-505.,-250.));
#6013=CARTESIAN_POINT('',(-799.,-533.,-250.));
#6014=CARTESIAN_POINT('',(-799.,-533.,-250.));
#6015=CARTESIAN_POINT('',(-801.,-535.,-250.));
#6016=CARTESIAN_POINT('Origin',(-801.,-533.,-250.));
#6017=CARTESIAN_POINT('',(-827.604006943529,-535.,-250.));
#6018=CARTESIAN_POINT('',(-801.,-535.,-250.));
#6019=CARTESIAN_POINT('',(-827.604006943529,-537.,-250.));
#6020=CARTESIAN_POINT('',(-827.604006943529,-535.,-250.));
#6021=CARTESIAN_POINT('',(-800.,-537.,-250.));
#6022=CARTESIAN_POINT('',(-800.,-537.,-250.));
#6023=CARTESIAN_POINT('',(-800.,-535.,-250.));
#6024=CARTESIAN_POINT('Origin',(250.,-505.,-250.));
#6025=CARTESIAN_POINT('',(-799.,-505.,250.));
#6026=CARTESIAN_POINT('',(-797.,-505.,250.));
#6027=CARTESIAN_POINT('Origin',(-799.,-505.,251.));
#6028=CARTESIAN_POINT('Origin',(-799.,-505.,-251.));
#6029=CARTESIAN_POINT('Origin',(250.,-505.,250.));
#6030=CARTESIAN_POINT('',(-799.,-533.,250.));
#6031=CARTESIAN_POINT('',(-801.,-535.,250.));
#6032=CARTESIAN_POINT('Origin',(-801.,-533.,250.));
#6033=CARTESIAN_POINT('',(-799.,-505.,250.));
#6034=CARTESIAN_POINT('',(-800.,-537.,250.));
#6035=CARTESIAN_POINT('',(-800.,-535.,250.));
#6036=CARTESIAN_POINT('',(-827.604006943529,-537.,250.));
#6037=CARTESIAN_POINT('',(-827.604006943529,-537.,250.));
#6038=CARTESIAN_POINT('',(-827.604006943529,-535.,250.));
#6039=CARTESIAN_POINT('',(-827.604006943529,-535.,250.));
#6040=CARTESIAN_POINT('',(-827.604006943529,-535.,250.));
#6041=CARTESIAN_POINT('Origin',(-725.,-534.,327.60400694353));
#6042=CARTESIAN_POINT('',(-827.604006943529,-535.,327.60400694353));
#6043=CARTESIAN_POINT('',(-725.,-535.,327.60400694353));
#6044=CARTESIAN_POINT('',(-827.604006943529,-537.,327.60400694353));
#6045=CARTESIAN_POINT('',(-827.604006943529,-535.,327.60400694353));
#6046=CARTESIAN_POINT('',(-725.,-537.,327.60400694353));
#6047=CARTESIAN_POINT('Origin',(-800.,-534.,300.));
#6048=CARTESIAN_POINT('',(-800.,-537.,300.));
#6049=CARTESIAN_POINT('',(-800.,-535.,300.));
#6050=CARTESIAN_POINT('',(-800.,-537.,300.));
#6051=CARTESIAN_POINT('Origin',(-800.,-534.,300.));
#6052=CARTESIAN_POINT('',(-800.,-537.,250.));
#6053=CARTESIAN_POINT('Origin',(-827.604006943529,-534.,327.60400694353));
#6054=CARTESIAN_POINT('',(-827.604006943529,-535.,327.60400694353));
#6055=CARTESIAN_POINT('',(-827.604006943529,-537.,327.60400694353));
#6056=CARTESIAN_POINT('Origin',(0.,-534.,0.));
#6057=CARTESIAN_POINT('',(-801.,-534.,251.));
#6058=CARTESIAN_POINT('',(-826.60400694353,-534.,251.));
#6059=CARTESIAN_POINT('',(-826.60400694353,-534.,251.));
#6060=CARTESIAN_POINT('',(-826.60400694353,-534.,326.60400694353));
#6061=CARTESIAN_POINT('',(-826.60400694353,-534.,326.60400694353));
#6062=CARTESIAN_POINT('',(-726.,-534.,326.60400694353));
#6063=CARTESIAN_POINT('',(-726.,-534.,326.60400694353));
#6064=CARTESIAN_POINT('',(-726.,-534.,301.));
#6065=CARTESIAN_POINT('',(-726.,-534.,301.));
#6066=CARTESIAN_POINT('',(-801.,-534.,301.));
#6067=CARTESIAN_POINT('',(-801.,-534.,301.));
#6068=CARTESIAN_POINT('',(-801.,-534.,251.));
#6069=CARTESIAN_POINT('Origin',(0.,-537.,0.));
#6070=CARTESIAN_POINT('Origin',(-800.,-534.,-300.));
#6071=CARTESIAN_POINT('',(-800.,-537.,-300.));
#6072=CARTESIAN_POINT('',(-800.,-535.,-300.));
#6073=CARTESIAN_POINT('',(-725.,-537.,-300.));
#6074=CARTESIAN_POINT('Origin',(-725.,-534.,-327.60400694353));
#6075=CARTESIAN_POINT('',(-827.604006943529,-535.,-327.60400694353));
#6076=CARTESIAN_POINT('',(-827.604006943529,-537.,-327.60400694353));
#6077=CARTESIAN_POINT('',(-827.604006943529,-535.,-327.60400694353));
#6078=CARTESIAN_POINT('',(-827.604006943529,-535.,-327.60400694353));
#6079=CARTESIAN_POINT('',(-827.604006943529,-537.,-327.60400694353));
#6080=CARTESIAN_POINT('Origin',(-827.604006943529,-534.,-327.60400694353));
#6081=CARTESIAN_POINT('',(-827.604006943529,-535.,-250.));
#6082=CARTESIAN_POINT('',(-827.604006943529,-537.,-250.));
#6083=CARTESIAN_POINT('Origin',(-800.,-534.,-300.));
#6084=CARTESIAN_POINT('',(-800.,-537.,-300.));
#6085=CARTESIAN_POINT('Origin',(0.,-534.,0.));
#6086=CARTESIAN_POINT('',(-826.60400694353,-534.,-251.));
#6087=CARTESIAN_POINT('',(-801.,-534.,-251.));
#6088=CARTESIAN_POINT('',(-801.,-534.,-251.));
#6089=CARTESIAN_POINT('',(-801.,-534.,-301.));
#6090=CARTESIAN_POINT('',(-801.,-534.,-301.));
#6091=CARTESIAN_POINT('',(-726.,-534.,-301.));
#6092=CARTESIAN_POINT('',(-726.,-534.,-301.));
#6093=CARTESIAN_POINT('',(-726.,-534.,-326.60400694353));
#6094=CARTESIAN_POINT('',(-726.,-534.,-326.60400694353));
#6095=CARTESIAN_POINT('',(-826.60400694353,-534.,-326.60400694353));
#6096=CARTESIAN_POINT('',(-826.60400694353,-534.,-326.60400694353));
#6097=CARTESIAN_POINT('',(-826.60400694353,-534.,-251.));
#6098=CARTESIAN_POINT('Origin',(0.,-537.,0.));
#6099=CARTESIAN_POINT('Origin',(250.,-534.,-300.));
#6100=CARTESIAN_POINT('',(250.,-537.,-300.));
#6101=CARTESIAN_POINT('',(250.,-535.,-300.));
#6102=CARTESIAN_POINT('',(250.,-537.,-250.));
#6103=CARTESIAN_POINT('Origin',(277.60400694353,-534.,-327.60400694353));
#6104=CARTESIAN_POINT('',(277.60400694353,-535.,-327.60400694353));
#6105=CARTESIAN_POINT('',(277.60400694353,-537.,-327.60400694353));
#6106=CARTESIAN_POINT('',(277.60400694353,-535.,-327.60400694353));
#6107=CARTESIAN_POINT('',(277.60400694353,-535.,-327.60400694353));
#6108=CARTESIAN_POINT('',(277.60400694353,-537.,-327.60400694353));
#6109=CARTESIAN_POINT('Origin',(175.,-534.,-327.60400694353));
#6110=CARTESIAN_POINT('',(175.,-535.,-327.60400694353));
#6111=CARTESIAN_POINT('',(175.,-537.,-327.60400694353));
#6112=CARTESIAN_POINT('Origin',(250.,-534.,-300.));
#6113=CARTESIAN_POINT('',(250.,-537.,-300.));
#6114=CARTESIAN_POINT('Origin',(0.,-534.,0.));
#6115=CARTESIAN_POINT('',(176.,-534.,-326.60400694353));
#6116=CARTESIAN_POINT('',(176.,-534.,-301.));
#6117=CARTESIAN_POINT('',(176.,-534.,-301.));
#6118=CARTESIAN_POINT('',(251.,-534.,-301.));
#6119=CARTESIAN_POINT('',(251.,-534.,-301.));
#6120=CARTESIAN_POINT('',(251.,-534.,-251.));
#6121=CARTESIAN_POINT('',(251.,-534.,-251.));
#6122=CARTESIAN_POINT('',(276.60400694353,-534.,-251.));
#6123=CARTESIAN_POINT('',(276.60400694353,-534.,-251.));
#6124=CARTESIAN_POINT('',(276.60400694353,-534.,-326.60400694353));
#6125=CARTESIAN_POINT('',(276.60400694353,-534.,-326.60400694353));
#6126=CARTESIAN_POINT('',(176.,-534.,-326.60400694353));
#6127=CARTESIAN_POINT('Origin',(0.,-537.,0.));
#6128=CARTESIAN_POINT('Origin',(250.,-534.,300.));
#6129=CARTESIAN_POINT('',(250.,-537.,300.));
#6130=CARTESIAN_POINT('',(250.,-535.,300.));
#6131=CARTESIAN_POINT('',(175.,-537.,300.));
#6132=CARTESIAN_POINT('Origin',(175.,-534.,327.60400694353));
#6133=CARTESIAN_POINT('',(277.60400694353,-535.,327.60400694353));
#6134=CARTESIAN_POINT('',(277.60400694353,-537.,327.60400694353));
#6135=CARTESIAN_POINT('',(277.60400694353,-535.,327.60400694353));
#6136=CARTESIAN_POINT('',(277.60400694353,-535.,327.60400694353));
#6137=CARTESIAN_POINT('',(277.60400694353,-537.,327.60400694353));
#6138=CARTESIAN_POINT('Origin',(277.60400694353,-534.,327.60400694353));
#6139=CARTESIAN_POINT('',(277.60400694353,-535.,250.));
#6140=CARTESIAN_POINT('',(277.60400694353,-537.,250.));
#6141=CARTESIAN_POINT('Origin',(250.,-534.,300.));
#6142=CARTESIAN_POINT('',(250.,-537.,300.));
#6143=CARTESIAN_POINT('Origin',(0.,-534.,0.));
#6144=CARTESIAN_POINT('',(276.60400694353,-534.,251.));
#6145=CARTESIAN_POINT('',(251.,-534.,251.));
#6146=CARTESIAN_POINT('',(251.,-534.,251.));
#6147=CARTESIAN_POINT('',(251.,-534.,301.));
#6148=CARTESIAN_POINT('',(251.,-534.,301.));
#6149=CARTESIAN_POINT('',(176.,-534.,301.));
#6150=CARTESIAN_POINT('',(176.,-534.,301.));
#6151=CARTESIAN_POINT('',(176.,-534.,326.60400694353));
#6152=CARTESIAN_POINT('',(176.,-534.,326.60400694353));
#6153=CARTESIAN_POINT('',(276.60400694353,-534.,326.60400694353));
#6154=CARTESIAN_POINT('',(276.60400694353,-534.,326.60400694353));
#6155=CARTESIAN_POINT('',(276.60400694353,-534.,251.));
#6156=CARTESIAN_POINT('Origin',(0.,-537.,0.));
#6157=CARTESIAN_POINT('Origin',(-355.,-534.,-300.));
#6158=CARTESIAN_POINT('',(-195.,-537.,-300.));
#6159=CARTESIAN_POINT('Origin',(-355.,-534.,-327.60400694353));
#6160=CARTESIAN_POINT('',(-355.,-537.,-327.60400694353));
#6161=CARTESIAN_POINT('',(-355.,-534.,-327.60400694353));
#6162=CARTESIAN_POINT('Origin',(0.,-534.,0.));
#6163=CARTESIAN_POINT('Origin',(0.,-537.,0.));
#6164=CARTESIAN_POINT('Origin',(-355.,-534.,327.60400694353));
#6165=CARTESIAN_POINT('',(-195.,-537.,327.60400694353));
#6166=CARTESIAN_POINT('',(-195.,-534.,327.60400694353));
#6167=CARTESIAN_POINT('Origin',(-355.,-534.,300.));
#6168=CARTESIAN_POINT('',(-355.,-537.,300.));
#6169=CARTESIAN_POINT('Origin',(0.,-534.,0.));
#6170=CARTESIAN_POINT('Origin',(0.,-537.,0.));
#6171=CARTESIAN_POINT('Origin',(-726.,-535.,-300.));
#6172=CARTESIAN_POINT('Origin',(-726.,-535.,-301.));
#6173=CARTESIAN_POINT('Origin',(-726.,-535.,-326.60400694353));
#6174=CARTESIAN_POINT('Origin',(-726.,-535.,-299.));
#6175=CARTESIAN_POINT('Origin',(-726.,-533.,-299.));
#6176=CARTESIAN_POINT('Origin',(-725.,-535.,-326.60400694353));
#6177=CARTESIAN_POINT('Origin',(-826.60400694353,-535.,-326.60400694353));
#6178=CARTESIAN_POINT('Origin',(-726.,-533.,-301.));
#6179=CARTESIAN_POINT('Origin',(-726.,-533.,-301.));
#6180=CARTESIAN_POINT('Origin',(-826.60400694353,-535.,-327.60400694353));
#6181=CARTESIAN_POINT('Origin',(-826.604006943529,-535.,-251.));
#6182=CARTESIAN_POINT('Origin',(-800.,-533.,-301.));
#6183=CARTESIAN_POINT('Origin',(-801.,-533.,-301.));
#6184=CARTESIAN_POINT('Origin',(250.,-535.,-251.));
#6185=CARTESIAN_POINT('Origin',(-801.,-535.,-251.));
#6186=CARTESIAN_POINT('Origin',(-801.,-533.,300.));
#6187=CARTESIAN_POINT('Origin',(-801.,-533.,-251.));
#6188=CARTESIAN_POINT('Origin',(-801.,-533.,-251.));
#6189=CARTESIAN_POINT('Origin',(-799.,-533.,-251.));
#6190=CARTESIAN_POINT('Origin',(-799.,-535.,-251.));
#6191=CARTESIAN_POINT('Origin',(250.,-535.,-251.));
#6192=CARTESIAN_POINT('Origin',(251.,-535.,-251.));
#6193=CARTESIAN_POINT('Origin',(276.60400694353,-535.,-251.));
#6194=CARTESIAN_POINT('Origin',(249.,-535.,-251.));
#6195=CARTESIAN_POINT('Origin',(249.,-533.,-251.));
#6196=CARTESIAN_POINT('Origin',(276.60400694353,-535.,-327.60400694353));
#6197=CARTESIAN_POINT('Origin',(276.60400694353,-535.,-326.60400694353));
#6198=CARTESIAN_POINT('Origin',(251.,-533.,-251.));
#6199=CARTESIAN_POINT('Origin',(251.,-533.,-251.));
#6200=CARTESIAN_POINT('Origin',(175.,-535.,-326.60400694353));
#6201=CARTESIAN_POINT('Origin',(176.,-535.,-326.60400694353));
#6202=CARTESIAN_POINT('Origin',(251.,-533.,300.));
#6203=CARTESIAN_POINT('Origin',(251.,-533.,-301.));
#6204=CARTESIAN_POINT('Origin',(176.,-535.,-300.));
#6205=CARTESIAN_POINT('Origin',(176.,-535.,-301.));
#6206=CARTESIAN_POINT('Origin',(-800.,-533.,-301.));
#6207=CARTESIAN_POINT('Origin',(176.,-533.,-301.));
#6208=CARTESIAN_POINT('Origin',(176.,-533.,-301.));
#6209=CARTESIAN_POINT('Origin',(176.,-533.,-299.));
#6210=CARTESIAN_POINT('Origin',(176.,-535.,-299.));
#6211=CARTESIAN_POINT('Origin',(176.,-535.,-300.));
#6212=CARTESIAN_POINT('Origin',(176.,-535.,301.));
#6213=CARTESIAN_POINT('Origin',(176.,-535.,326.60400694353));
#6214=CARTESIAN_POINT('Origin',(176.,-505.,299.));
#6215=CARTESIAN_POINT('Origin',(176.,-533.,299.));
#6216=CARTESIAN_POINT('Origin',(175.,-535.,326.60400694353));
#6217=CARTESIAN_POINT('Origin',(276.60400694353,-535.,326.60400694353));
#6218=CARTESIAN_POINT('Origin',(176.,-533.,301.));
#6219=CARTESIAN_POINT('Origin',(176.,-533.,301.));
#6220=CARTESIAN_POINT('Origin',(276.60400694353,-535.,327.60400694353));
#6221=CARTESIAN_POINT('Origin',(276.60400694353,-535.,251.));
#6222=CARTESIAN_POINT('Origin',(-800.,-533.,301.));
#6223=CARTESIAN_POINT('Origin',(251.,-533.,301.));
#6224=CARTESIAN_POINT('Origin',(250.,-535.,251.));
#6225=CARTESIAN_POINT('Origin',(251.,-535.,251.));
#6226=CARTESIAN_POINT('Origin',(251.,-533.,300.));
#6227=CARTESIAN_POINT('Origin',(251.,-533.,251.));
#6228=CARTESIAN_POINT('Origin',(251.,-533.,251.));
#6229=CARTESIAN_POINT('Origin',(249.,-533.,251.));
#6230=CARTESIAN_POINT('Origin',(249.,-535.,251.));
#6231=CARTESIAN_POINT('Origin',(-726.,-505.,299.));
#6232=CARTESIAN_POINT('Origin',(-726.,-533.,299.));
#6233=CARTESIAN_POINT('Origin',(-726.,-535.,-300.));
#6234=CARTESIAN_POINT('Origin',(-726.,-535.,326.60400694353));
#6235=CARTESIAN_POINT('Origin',(-726.,-535.,301.));
#6236=CARTESIAN_POINT('Origin',(-726.,-533.,301.));
#6237=CARTESIAN_POINT('Origin',(-726.,-533.,301.));
#6238=CARTESIAN_POINT('Origin',(-725.,-535.,326.60400694353));
#6239=CARTESIAN_POINT('Origin',(-826.60400694353,-535.,326.60400694353));
#6240=CARTESIAN_POINT('Origin',(-800.,-533.,301.));
#6241=CARTESIAN_POINT('Origin',(-801.,-533.,301.));
#6242=CARTESIAN_POINT('Origin',(-826.60400694353,-535.,327.60400694353));
#6243=CARTESIAN_POINT('Origin',(-826.604006943529,-535.,251.));
#6244=CARTESIAN_POINT('Origin',(-801.,-533.,300.));
#6245=CARTESIAN_POINT('Origin',(-801.,-533.,251.));
#6246=CARTESIAN_POINT('Origin',(250.,-535.,251.));
#6247=CARTESIAN_POINT('Origin',(-801.,-535.,251.));
#6248=CARTESIAN_POINT('Origin',(-801.,-533.,251.));
#6249=CARTESIAN_POINT('Origin',(-799.,-533.,251.));
#6250=CARTESIAN_POINT('Origin',(-799.,-535.,251.));
#6251=CARTESIAN_POINT('Origin',(0.,175.,0.));
#6252=CARTESIAN_POINT('',(-4.28626379701574E-15,175.,35.));
#6253=CARTESIAN_POINT('Origin',(-500.,175.,-6.12323399573677E-14));
#6254=CARTESIAN_POINT('',(-500.,175.,35.));
#6255=CARTESIAN_POINT('',(0.,0.,0.));
#6256=CARTESIAN_POINT('Origin',(-135.,-310.693069306929,302.));
#6257=CARTESIAN_POINT('',(-135.,-310.693069306929,300.));
#6258=CARTESIAN_POINT('',(-135.,-505.693069306929,300.));
#6259=CARTESIAN_POINT('',(-135.,-310.693069306929,300.));
#6260=CARTESIAN_POINT('',(-135.,-505.693069306929,302.));
#6261=CARTESIAN_POINT('',(-135.,-505.693069306929,302.));
#6262=CARTESIAN_POINT('',(-135.,-310.693069306929,302.));
#6263=CARTESIAN_POINT('',(-135.,-310.693069306929,302.));
#6264=CARTESIAN_POINT('',(-135.,-310.693069306929,302.));
#6265=CARTESIAN_POINT('Origin',(-135.,-505.693069306929,302.));
#6266=CARTESIAN_POINT('',(225.,-505.693069306929,300.));
#6267=CARTESIAN_POINT('',(-135.,-505.693069306929,300.));
#6268=CARTESIAN_POINT('',(225.,-505.693069306929,302.));
#6269=CARTESIAN_POINT('',(225.,-505.693069306929,302.));
#6270=CARTESIAN_POINT('',(-135.,-505.693069306929,302.));
#6271=CARTESIAN_POINT('Origin',(225.,-310.693069306929,302.));
#6272=CARTESIAN_POINT('',(225.,-310.693069306929,300.));
#6273=CARTESIAN_POINT('',(225.,-310.693069306929,300.));
#6274=CARTESIAN_POINT('',(225.,-310.693069306929,302.));
#6275=CARTESIAN_POINT('',(225.,-310.693069306929,302.));
#6276=CARTESIAN_POINT('',(225.,-310.693069306929,302.));
#6277=CARTESIAN_POINT('Origin',(-135.,-310.693069306929,302.));
#6278=CARTESIAN_POINT('',(-135.,-310.693069306929,300.));
#6279=CARTESIAN_POINT('',(-135.,-310.693069306929,302.));
#6280=CARTESIAN_POINT('Origin',(0.,0.,302.));
#6281=CARTESIAN_POINT('',(-62.9999999999999,-400.193069306929,302.));
#6282=CARTESIAN_POINT('',(-62.9999999999999,-416.193069306929,302.));
#6283=CARTESIAN_POINT('Origin',(-62.9999999999999,-408.193069306929,302.));
#6284=CARTESIAN_POINT('',(153.,-400.193069306929,302.));
#6285=CARTESIAN_POINT('',(153.,-400.193069306929,302.));
#6286=CARTESIAN_POINT('',(153.,-416.193069306929,302.));
#6287=CARTESIAN_POINT('Origin',(153.,-408.193069306929,302.));
#6288=CARTESIAN_POINT('',(-62.9999999999999,-416.193069306929,302.));
#6289=CARTESIAN_POINT('',(-63.,-370.193069306929,302.));
#6290=CARTESIAN_POINT('',(-63.,-386.193069306929,302.));
#6291=CARTESIAN_POINT('Origin',(-63.,-378.193069306929,302.));
#6292=CARTESIAN_POINT('',(153.,-370.193069306929,302.));
#6293=CARTESIAN_POINT('',(153.,-370.193069306929,302.));
#6294=CARTESIAN_POINT('',(153.,-386.193069306929,302.));
#6295=CARTESIAN_POINT('Origin',(153.,-378.193069306929,302.));
#6296=CARTESIAN_POINT('',(-63.,-386.193069306929,302.));
#6297=CARTESIAN_POINT('',(-63.0000000000001,-340.193069306929,302.));
#6298=CARTESIAN_POINT('',(-63.0000000000001,-356.193069306929,302.));
#6299=CARTESIAN_POINT('Origin',(-63.0000000000001,-348.193069306929,302.));
#6300=CARTESIAN_POINT('',(153.,-340.193069306929,302.));
#6301=CARTESIAN_POINT('',(153.,-340.193069306929,302.));
#6302=CARTESIAN_POINT('',(153.,-356.193069306929,302.));
#6303=CARTESIAN_POINT('Origin',(153.,-348.193069306929,302.));
#6304=CARTESIAN_POINT('',(-63.0000000000001,-356.193069306929,302.));
#6305=CARTESIAN_POINT('',(-62.9999999999996,-430.193069306929,302.));
#6306=CARTESIAN_POINT('',(-62.9999999999996,-446.193069306929,302.));
#6307=CARTESIAN_POINT('Origin',(-62.9999999999996,-438.193069306929,302.));
#6308=CARTESIAN_POINT('',(153.,-430.193069306929,302.));
#6309=CARTESIAN_POINT('',(153.,-430.193069306929,302.));
#6310=CARTESIAN_POINT('',(153.,-446.193069306929,302.));
#6311=CARTESIAN_POINT('Origin',(153.,-438.193069306929,302.));
#6312=CARTESIAN_POINT('',(-62.9999999999996,-446.193069306929,302.));
#6313=CARTESIAN_POINT('',(-62.9999999999993,-460.193069306929,302.));
#6314=CARTESIAN_POINT('',(-62.9999999999993,-476.193069306929,302.));
#6315=CARTESIAN_POINT('Origin',(-62.9999999999993,-468.193069306929,302.));
#6316=CARTESIAN_POINT('',(153.000000000001,-460.193069306928,302.));
#6317=CARTESIAN_POINT('',(153.000000000001,-460.193069306928,302.));
#6318=CARTESIAN_POINT('',(153.000000000001,-476.193069306929,302.));
#6319=CARTESIAN_POINT('Origin',(153.000000000001,-468.193069306929,302.));
#6320=CARTESIAN_POINT('',(-62.9999999999993,-476.193069306929,302.));
#6321=CARTESIAN_POINT('',(208.,-325.693069306929,302.));
#6322=CARTESIAN_POINT('Origin',(210.,-325.693069306929,302.));
#6323=CARTESIAN_POINT('',(-122.,-325.693069306929,302.));
#6324=CARTESIAN_POINT('Origin',(-120.,-325.693069306929,302.));
#6325=CARTESIAN_POINT('',(208.,-490.693069306929,302.));
#6326=CARTESIAN_POINT('Origin',(210.,-490.693069306929,302.));
#6327=CARTESIAN_POINT('',(-122.,-490.693069306929,302.));
#6328=CARTESIAN_POINT('Origin',(-120.,-490.693069306929,302.));
#6329=CARTESIAN_POINT('Origin',(0.,0.,300.));
#6330=CARTESIAN_POINT('',(153.,-400.193069306929,300.));
#6331=CARTESIAN_POINT('',(-62.9999999999999,-400.193069306929,300.));
#6332=CARTESIAN_POINT('',(153.,-400.193069306929,300.));
#6333=CARTESIAN_POINT('',(-62.9999999999999,-416.193069306929,300.));
#6334=CARTESIAN_POINT('Origin',(-62.9999999999999,-408.193069306929,300.));
#6335=CARTESIAN_POINT('',(153.,-416.193069306929,300.));
#6336=CARTESIAN_POINT('',(-62.9999999999999,-416.193069306929,300.));
#6337=CARTESIAN_POINT('Origin',(153.,-408.193069306929,300.));
#6338=CARTESIAN_POINT('',(153.,-370.193069306929,300.));
#6339=CARTESIAN_POINT('',(-63.,-370.193069306929,300.));
#6340=CARTESIAN_POINT('',(153.,-370.193069306929,300.));
#6341=CARTESIAN_POINT('',(-63.,-386.193069306929,300.));
#6342=CARTESIAN_POINT('Origin',(-63.,-378.193069306929,300.));
#6343=CARTESIAN_POINT('',(153.,-386.193069306929,300.));
#6344=CARTESIAN_POINT('',(-63.,-386.193069306929,300.));
#6345=CARTESIAN_POINT('Origin',(153.,-378.193069306929,300.));
#6346=CARTESIAN_POINT('',(153.,-340.193069306929,300.));
#6347=CARTESIAN_POINT('',(-63.0000000000001,-340.193069306929,300.));
#6348=CARTESIAN_POINT('',(153.,-340.193069306929,300.));
#6349=CARTESIAN_POINT('',(-63.0000000000001,-356.193069306929,300.));
#6350=CARTESIAN_POINT('Origin',(-63.0000000000001,-348.193069306929,300.));
#6351=CARTESIAN_POINT('',(153.,-356.193069306929,300.));
#6352=CARTESIAN_POINT('',(-63.0000000000001,-356.193069306929,300.));
#6353=CARTESIAN_POINT('Origin',(153.,-348.193069306929,300.));
#6354=CARTESIAN_POINT('',(153.,-430.193069306929,300.));
#6355=CARTESIAN_POINT('',(-62.9999999999996,-430.193069306929,300.));
#6356=CARTESIAN_POINT('',(153.,-430.193069306929,300.));
#6357=CARTESIAN_POINT('',(-62.9999999999996,-446.193069306929,300.));
#6358=CARTESIAN_POINT('Origin',(-62.9999999999996,-438.193069306929,300.));
#6359=CARTESIAN_POINT('',(153.,-446.193069306929,300.));
#6360=CARTESIAN_POINT('',(-62.9999999999996,-446.193069306929,300.));
#6361=CARTESIAN_POINT('Origin',(153.,-438.193069306929,300.));
#6362=CARTESIAN_POINT('',(153.000000000001,-460.193069306928,300.));
#6363=CARTESIAN_POINT('',(-62.9999999999993,-460.193069306929,300.));
#6364=CARTESIAN_POINT('',(153.000000000001,-460.193069306928,300.));
#6365=CARTESIAN_POINT('',(-62.9999999999993,-476.193069306929,300.));
#6366=CARTESIAN_POINT('Origin',(-62.9999999999993,-468.193069306929,300.));
#6367=CARTESIAN_POINT('',(153.000000000001,-476.193069306929,300.));
#6368=CARTESIAN_POINT('',(-62.9999999999993,-476.193069306929,300.));
#6369=CARTESIAN_POINT('Origin',(153.000000000001,-468.193069306929,300.));
#6370=CARTESIAN_POINT('',(208.,-325.693069306929,300.));
#6371=CARTESIAN_POINT('Origin',(210.,-325.693069306929,300.));
#6372=CARTESIAN_POINT('',(-122.,-325.693069306929,300.));
#6373=CARTESIAN_POINT('Origin',(-120.,-325.693069306929,300.));
#6374=CARTESIAN_POINT('',(208.,-490.693069306929,300.));
#6375=CARTESIAN_POINT('Origin',(210.,-490.693069306929,300.));
#6376=CARTESIAN_POINT('',(-122.,-490.693069306929,300.));
#6377=CARTESIAN_POINT('Origin',(-120.,-490.693069306929,300.));
#6378=CARTESIAN_POINT('Origin',(-120.,-490.693069306929,280.));
#6379=CARTESIAN_POINT('',(-122.,-490.693069306929,280.));
#6380=CARTESIAN_POINT('Origin',(210.,-490.693069306929,280.));
#6381=CARTESIAN_POINT('',(208.,-490.693069306929,280.));
#6382=CARTESIAN_POINT('Origin',(-120.,-325.693069306929,280.));
#6383=CARTESIAN_POINT('',(-122.,-325.693069306929,280.));
#6384=CARTESIAN_POINT('Origin',(210.,-325.693069306929,280.));
#6385=CARTESIAN_POINT('',(208.,-325.693069306929,280.));
#6386=CARTESIAN_POINT('Origin',(-62.9999999999993,-468.193069306929,280.));
#6387=CARTESIAN_POINT('',(-62.9999999999993,-460.193069306929,300.));
#6388=CARTESIAN_POINT('',(-62.9999999999993,-476.193069306929,300.));
#6389=CARTESIAN_POINT('Origin',(-62.9999999999993,-460.193069306929,280.));
#6390=CARTESIAN_POINT('',(153.000000000001,-460.193069306928,300.));
#6391=CARTESIAN_POINT('Origin',(153.000000000001,-468.193069306929,280.));
#6392=CARTESIAN_POINT('',(153.000000000001,-476.193069306929,300.));
#6393=CARTESIAN_POINT('Origin',(-62.9999999999993,-476.193069306929,280.));
#6394=CARTESIAN_POINT('Origin',(-62.9999999999996,-438.193069306929,280.));
#6395=CARTESIAN_POINT('',(-62.9999999999996,-430.193069306929,300.));
#6396=CARTESIAN_POINT('',(-62.9999999999996,-446.193069306929,300.));
#6397=CARTESIAN_POINT('Origin',(-62.9999999999996,-430.193069306929,280.));
#6398=CARTESIAN_POINT('',(153.,-430.193069306929,300.));
#6399=CARTESIAN_POINT('Origin',(153.,-438.193069306929,280.));
#6400=CARTESIAN_POINT('',(153.,-446.193069306929,300.));
#6401=CARTESIAN_POINT('Origin',(-62.9999999999996,-446.193069306929,280.));
#6402=CARTESIAN_POINT('Origin',(-63.0000000000001,-348.193069306929,280.));
#6403=CARTESIAN_POINT('',(-63.0000000000001,-340.193069306929,300.));
#6404=CARTESIAN_POINT('',(-63.0000000000001,-356.193069306929,300.));
#6405=CARTESIAN_POINT('Origin',(-63.0000000000001,-340.193069306929,280.));
#6406=CARTESIAN_POINT('',(153.,-340.193069306929,300.));
#6407=CARTESIAN_POINT('Origin',(153.,-348.193069306929,280.));
#6408=CARTESIAN_POINT('',(153.,-356.193069306929,300.));
#6409=CARTESIAN_POINT('Origin',(-63.0000000000001,-356.193069306929,280.));
#6410=CARTESIAN_POINT('Origin',(-63.,-378.193069306929,280.));
#6411=CARTESIAN_POINT('',(-63.,-370.193069306929,300.));
#6412=CARTESIAN_POINT('',(-63.,-386.193069306929,300.));
#6413=CARTESIAN_POINT('Origin',(-63.,-370.193069306929,280.));
#6414=CARTESIAN_POINT('',(153.,-370.193069306929,300.));
#6415=CARTESIAN_POINT('Origin',(153.,-378.193069306929,280.));
#6416=CARTESIAN_POINT('',(153.,-386.193069306929,300.));
#6417=CARTESIAN_POINT('Origin',(-63.,-386.193069306929,280.));
#6418=CARTESIAN_POINT('Origin',(-62.9999999999999,-408.193069306929,280.));
#6419=CARTESIAN_POINT('',(-62.9999999999999,-400.193069306929,300.));
#6420=CARTESIAN_POINT('',(-62.9999999999999,-416.193069306929,300.));
#6421=CARTESIAN_POINT('Origin',(-62.9999999999999,-400.193069306929,280.));
#6422=CARTESIAN_POINT('',(153.,-400.193069306929,300.));
#6423=CARTESIAN_POINT('Origin',(153.,-408.193069306929,280.));
#6424=CARTESIAN_POINT('',(153.,-416.193069306929,300.));
#6425=CARTESIAN_POINT('Origin',(-62.9999999999999,-416.193069306929,280.));
#6426=CARTESIAN_POINT('',(275.,537.,0.));
#6427=CARTESIAN_POINT('',(275.,537.,0.));
#6428=CARTESIAN_POINT('',(-275.,537.,602.));
#6429=CARTESIAN_POINT('',(0.,0.,0.));
#6430=CARTESIAN_POINT('Origin',(0.,42.0000000000001,0.));
#6431=CARTESIAN_POINT('',(-3.06161699786838E-15,-388.,25.));
#6432=CARTESIAN_POINT('Origin',(0.,-388.,0.));
#6433=CARTESIAN_POINT('',(-3.06161699786838E-15,-15.,25.));
#6434=CARTESIAN_POINT('',(-3.06161699786838E-15,42.0000000000001,25.));
#6435=CARTESIAN_POINT('',(-1.5,-15.,24.9549594269356));
#6436=CARTESIAN_POINT('Origin',(0.,-15.,0.));
#6437=CARTESIAN_POINT('',(-1.5,42.0000000000001,24.9549594269356));
#6438=CARTESIAN_POINT('',(-1.5,-15.,24.9549594269356));
#6439=CARTESIAN_POINT('',(-1.5,42.0000000000001,-24.9549594269356));
#6440=CARTESIAN_POINT('Origin',(0.,42.0000000000001,0.));
#6441=CARTESIAN_POINT('',(-1.5,-15.,-24.9549594269356));
#6442=CARTESIAN_POINT('',(-1.49999999999999,-15.,-24.9549594269356));
#6443=CARTESIAN_POINT('',(1.5,-15.,-24.9549594269356));
#6444=CARTESIAN_POINT('Origin',(0.,-15.,0.));
#6445=CARTESIAN_POINT('',(1.5,42.0000000000001,-24.9549594269356));
#6446=CARTESIAN_POINT('',(1.5,-15.,-24.9549594269356));
#6447=CARTESIAN_POINT('',(1.5,42.0000000000001,24.9549594269356));
#6448=CARTESIAN_POINT('Origin',(0.,42.0000000000001,0.));
#6449=CARTESIAN_POINT('',(1.5,-15.,24.9549594269356));
#6450=CARTESIAN_POINT('',(1.5,-15.,24.9549594269356));
#6451=CARTESIAN_POINT('Origin',(0.,-15.,0.));
#6452=CARTESIAN_POINT('Origin',(0.,42.0000000000001,0.));
#6453=CARTESIAN_POINT('',(1.5,42.0000000000001,-30.));
#6454=CARTESIAN_POINT('',(1.5,42.0000000000001,-24.9549594269356));
#6455=CARTESIAN_POINT('',(-1.5,42.0000000000001,-30.));
#6456=CARTESIAN_POINT('',(1.5,42.0000000000001,-30.));
#6457=CARTESIAN_POINT('',(-1.5,42.0000000000001,-30.));
#6458=CARTESIAN_POINT('',(-1.5,42.0000000000001,30.));
#6459=CARTESIAN_POINT('',(-1.5,42.0000000000001,24.9549594269356));
#6460=CARTESIAN_POINT('',(1.5,42.0000000000001,30.));
#6461=CARTESIAN_POINT('',(-1.5,42.0000000000001,30.));
#6462=CARTESIAN_POINT('',(1.5,42.0000000000001,30.));
#6463=CARTESIAN_POINT('',(-9.18485099360515E-16,42.0000000000001,-7.5));
#6464=CARTESIAN_POINT('Origin',(0.,42.0000000000001,0.));
#6465=CARTESIAN_POINT('Origin',(0.,-388.,0.));
#6466=CARTESIAN_POINT('Origin',(0.,-15.,0.));
#6467=CARTESIAN_POINT('',(-1.5,-15.,30.));
#6468=CARTESIAN_POINT('',(1.5,-15.,30.));
#6469=CARTESIAN_POINT('',(-1.5,-15.,30.));
#6470=CARTESIAN_POINT('',(-1.5,-15.,24.9549594269356));
#6471=CARTESIAN_POINT('',(1.5,-15.,30.));
#6472=CARTESIAN_POINT('Origin',(1.5,-20.8696196115137,30.));
#6473=CARTESIAN_POINT('',(1.5,-15.,30.));
#6474=CARTESIAN_POINT('Origin',(-1.5,-20.8696196115137,30.));
#6475=CARTESIAN_POINT('',(-1.5,-15.,30.));
#6476=CARTESIAN_POINT('Origin',(-1.5,-20.8696196115137,30.));
#6477=CARTESIAN_POINT('Origin',(0.,-15.,0.));
#6478=CARTESIAN_POINT('',(-1.5,-15.,-30.));
#6479=CARTESIAN_POINT('',(-1.5,-15.,-30.));
#6480=CARTESIAN_POINT('',(1.5,-15.,-30.));
#6481=CARTESIAN_POINT('',(1.5,-15.,-30.));
#6482=CARTESIAN_POINT('',(1.5,-15.,-24.9549594269356));
#6483=CARTESIAN_POINT('Origin',(1.5,-20.8696196115137,-30.));
#6484=CARTESIAN_POINT('',(1.5,-15.,-30.));
#6485=CARTESIAN_POINT('Origin',(-1.5,-20.8696196115137,-30.));
#6486=CARTESIAN_POINT('',(-1.5,-15.,-30.));
#6487=CARTESIAN_POINT('Origin',(-1.5,-20.8696196115137,-30.));
#6488=CARTESIAN_POINT('Origin',(0.,42.0000000000001,0.));
#6489=CARTESIAN_POINT('',(-5.97056964114407E-16,12.0000000000001,-4.87534009422228));
#6490=CARTESIAN_POINT('Origin',(0.,12.0000000000001,0.));
#6491=CARTESIAN_POINT('',(-9.18485099360515E-16,42.0000000000001,-7.5));
#6492=CARTESIAN_POINT('Origin',(0.,12.0000000000001,0.));
#6493=CARTESIAN_POINT('',(0.,0.,0.));
#6494=CARTESIAN_POINT('Origin',(0.,0.,0.));
#6495=CARTESIAN_POINT('',(3.01869176962471,0.,21.95));
#6496=CARTESIAN_POINT('',(3.01869176962471,-2.68809972412844E-15,-21.95));
#6497=CARTESIAN_POINT('Origin',(3.01869176962471,0.,0.));
#6498=CARTESIAN_POINT('',(3.01869176962472,-2.02679045258887E-15,-16.55));
#6499=CARTESIAN_POINT('Origin',(0.,-2.35744508835865E-15,-19.25));
#6500=CARTESIAN_POINT('',(3.01869176962472,0.,16.55));
#6501=CARTESIAN_POINT('Origin',(3.01869176962472,0.,0.));
#6502=CARTESIAN_POINT('Origin',(3.01869176962472,0.,0.));
#6503=CARTESIAN_POINT('Origin',(3.01869176962471,0.,0.));
#6504=CARTESIAN_POINT('Origin',(-20.6375,0.,0.));
#6505=CARTESIAN_POINT('',(9.,-2.02679045258887E-15,16.55));
#6506=CARTESIAN_POINT('Origin',(9.,0.,0.));
#6507=CARTESIAN_POINT('',(-20.6375,-2.02679045258887E-15,16.55));
#6508=CARTESIAN_POINT('Origin',(-20.6375,0.,0.));
#6509=CARTESIAN_POINT('',(-3.01869176962472,0.,-16.55));
#6510=CARTESIAN_POINT('',(-3.01869176962472,-2.02679045258887E-15,16.55));
#6511=CARTESIAN_POINT('Origin',(-3.01869176962472,0.,0.));
#6512=CARTESIAN_POINT('Origin',(-3.01869176962472,0.,0.));
#6513=CARTESIAN_POINT('',(-9.,-2.02679045258887E-15,16.55));
#6514=CARTESIAN_POINT('',(-20.6375,-2.02679045258887E-15,16.55));
#6515=CARTESIAN_POINT('Origin',(-9.,0.,0.));
#6516=CARTESIAN_POINT('Origin',(9.,13.5,0.));
#6517=CARTESIAN_POINT('',(9.,-1.65327317884893E-15,13.5));
#6518=CARTESIAN_POINT('Origin',(9.,0.,0.));
#6519=CARTESIAN_POINT('Origin',(8.,0.,0.));
#6520=CARTESIAN_POINT('',(8.,-1.53080849893419E-15,12.5));
#6521=CARTESIAN_POINT('Origin',(8.,0.,0.));
#6522=CARTESIAN_POINT('Origin',(8.,-1.65327317884893E-15,13.5));
#6523=CARTESIAN_POINT('Origin',(-20.6375,0.,0.));
#6524=CARTESIAN_POINT('',(-8.,-1.53080849893419E-15,12.5));
#6525=CARTESIAN_POINT('Origin',(-8.,0.,0.));
#6526=CARTESIAN_POINT('',(-20.6375,-1.53080849893419E-15,12.5));
#6527=CARTESIAN_POINT('Origin',(-8.,0.,0.));
#6528=CARTESIAN_POINT('',(-9.,-1.65327317884893E-15,13.5));
#6529=CARTESIAN_POINT('Origin',(-9.,0.,0.));
#6530=CARTESIAN_POINT('Origin',(-8.,-1.65327317884893E-15,13.5));
#6531=CARTESIAN_POINT('Origin',(-9.,16.55,0.));
#6532=CARTESIAN_POINT('Origin',(0.,0.,0.));
#6533=CARTESIAN_POINT('',(-3.01869176962471,0.,-21.95));
#6534=CARTESIAN_POINT('Origin',(0.,-2.35744508835865E-15,-19.25));
#6535=CARTESIAN_POINT('',(-3.01869176962471,-2.68809972412844E-15,21.95));
#6536=CARTESIAN_POINT('Origin',(-3.01869176962471,0.,0.));
#6537=CARTESIAN_POINT('Origin',(-3.01869176962471,0.,0.));
#6538=CARTESIAN_POINT('Origin',(-20.6375,0.,0.));
#6539=CARTESIAN_POINT('',(9.,-2.68809972412844E-15,21.95));
#6540=CARTESIAN_POINT('',(-20.6375,-2.68809972412844E-15,21.95));
#6541=CARTESIAN_POINT('Origin',(9.,0.,0.));
#6542=CARTESIAN_POINT('Origin',(-20.6375,0.,0.));
#6543=CARTESIAN_POINT('',(-9.,-2.68809972412844E-15,21.95));
#6544=CARTESIAN_POINT('Origin',(-9.,0.,0.));
#6545=CARTESIAN_POINT('',(-20.6375,-2.68809972412844E-15,21.95));
#6546=CARTESIAN_POINT('Origin',(9.,25.,0.));
#6547=CARTESIAN_POINT('',(9.,-3.06161699786838E-15,25.));
#6548=CARTESIAN_POINT('Origin',(9.,0.,0.));
#6549=CARTESIAN_POINT('Origin',(8.,0.,0.));
#6550=CARTESIAN_POINT('',(8.,-3.18408167778312E-15,26.));
#6551=CARTESIAN_POINT('Origin',(8.,-3.06161699786838E-15,25.));
#6552=CARTESIAN_POINT('Origin',(8.,0.,0.));
#6553=CARTESIAN_POINT('Origin',(-20.6375,0.,0.));
#6554=CARTESIAN_POINT('',(-8.,-3.18408167778312E-15,26.));
#6555=CARTESIAN_POINT('',(-20.6375,-3.18408167778312E-15,26.));
#6556=CARTESIAN_POINT('Origin',(-8.,0.,0.));
#6557=CARTESIAN_POINT('Origin',(-8.,0.,0.));
#6558=CARTESIAN_POINT('',(-9.,-3.06161699786838E-15,25.));
#6559=CARTESIAN_POINT('Origin',(-8.,-3.06161699786838E-15,25.));
#6560=CARTESIAN_POINT('Origin',(-9.,0.,0.));
#6561=CARTESIAN_POINT('Origin',(-9.,21.95,0.));
#6562=CARTESIAN_POINT('',(0.,0.,0.));
#6563=CARTESIAN_POINT('Origin',(0.,0.,15.));
#6564=CARTESIAN_POINT('',(130.,0.,-15.));
#6565=CARTESIAN_POINT('Origin',(0.,0.,-15.));
#6566=CARTESIAN_POINT('',(130.,0.,-12.));
#6567=CARTESIAN_POINT('',(130.,-1.59204083889156E-14,15.));
#6568=CARTESIAN_POINT('Origin',(0.,0.,-12.));
#6569=CARTESIAN_POINT('Origin',(0.,0.,15.));
#6570=CARTESIAN_POINT('',(130.,0.,12.));
#6571=CARTESIAN_POINT('',(-130.,-1.59204083889156E-14,12.));
#6572=CARTESIAN_POINT('Origin',(0.,0.,12.));
#6573=CARTESIAN_POINT('Origin',(0.,0.,12.));
#6574=CARTESIAN_POINT('',(130.,0.,15.));
#6575=CARTESIAN_POINT('',(130.,-1.59204083889156E-14,15.));
#6576=CARTESIAN_POINT('Origin',(0.,0.,15.));
#6577=CARTESIAN_POINT('Origin',(51.0954988232815,29.5000000000006,-15.));
#6578=CARTESIAN_POINT('',(48.5954988232815,33.8301270189228,-5.));
#6579=CARTESIAN_POINT('Origin',(51.0954988232815,29.5000000000006,-5.));
#6580=CARTESIAN_POINT('',(48.5954988232815,33.8301270189228,5.));
#6581=CARTESIAN_POINT('',(48.5954988232815,33.8301270189228,-15.));
#6582=CARTESIAN_POINT('Origin',(51.0954988232815,29.5000000000006,5.));
#6583=CARTESIAN_POINT('Origin',(51.0954988232822,-29.4999999999995,-15.));
#6584=CARTESIAN_POINT('',(53.5954988232821,-25.1698729810773,-5.));
#6585=CARTESIAN_POINT('Origin',(51.0954988232822,-29.4999999999995,-5.));
#6586=CARTESIAN_POINT('',(53.5954988232821,-25.1698729810773,5.));
#6587=CARTESIAN_POINT('',(53.5954988232821,-25.1698729810773,-15.));
#6588=CARTESIAN_POINT('Origin',(51.0954988232822,-29.4999999999995,5.));
#6589=CARTESIAN_POINT('Origin',(0.,-59.,-15.));
#6590=CARTESIAN_POINT('',(5.,-59.,-5.));
#6591=CARTESIAN_POINT('Origin',(0.,-59.,-5.));
#6592=CARTESIAN_POINT('',(5.,-59.,5.));
#6593=CARTESIAN_POINT('',(5.,-59.,-15.));
#6594=CARTESIAN_POINT('Origin',(0.,-59.,5.));
#6595=CARTESIAN_POINT('Origin',(-51.0954988232818,-29.5000000000002,-15.));
#6596=CARTESIAN_POINT('',(-48.5954988232817,-33.8301270189224,-5.));
#6597=CARTESIAN_POINT('Origin',(-51.0954988232818,-29.5000000000002,-5.));
#6598=CARTESIAN_POINT('',(-48.5954988232817,-33.8301270189224,5.));
#6599=CARTESIAN_POINT('',(-48.5954988232817,-33.8301270189224,-15.));
#6600=CARTESIAN_POINT('Origin',(-51.0954988232818,-29.5000000000002,5.));
#6601=CARTESIAN_POINT('Origin',(-51.095498823282,29.4999999999999,-15.));
#6602=CARTESIAN_POINT('',(-53.5954988232819,25.1698729810777,-5.));
#6603=CARTESIAN_POINT('Origin',(-51.095498823282,29.4999999999999,-5.));
#6604=CARTESIAN_POINT('',(-53.5954988232819,25.1698729810777,5.));
#6605=CARTESIAN_POINT('',(-53.5954988232819,25.1698729810777,-15.));
#6606=CARTESIAN_POINT('Origin',(-51.095498823282,29.4999999999999,5.));
#6607=CARTESIAN_POINT('Origin',(0.,0.,15.));
#6608=CARTESIAN_POINT('',(90.,0.,-5.));
#6609=CARTESIAN_POINT('Origin',(0.,0.,-5.));
#6610=CARTESIAN_POINT('',(90.,0.,-15.));
#6611=CARTESIAN_POINT('',(90.,-1.10218211923262E-14,15.));
#6612=CARTESIAN_POINT('Origin',(0.,0.,-15.));
#6613=CARTESIAN_POINT('Origin',(0.,0.,15.));
#6614=CARTESIAN_POINT('',(90.,0.,15.));
#6615=CARTESIAN_POINT('Origin',(0.,0.,15.));
#6616=CARTESIAN_POINT('',(90.,0.,5.));
#6617=CARTESIAN_POINT('',(90.,-1.10218211923262E-14,15.));
#6618=CARTESIAN_POINT('Origin',(0.,0.,5.));
#6619=CARTESIAN_POINT('Origin',(0.,0.,15.));
#6620=CARTESIAN_POINT('Origin',(0.,0.,-15.));
#6621=CARTESIAN_POINT('Origin',(0.,0.,5.));
#6622=CARTESIAN_POINT('',(-5.,59.,5.));
#6623=CARTESIAN_POINT('Origin',(0.,59.,5.));
#6624=CARTESIAN_POINT('',(28.,0.,5.));
#6625=CARTESIAN_POINT('Origin',(0.,0.,5.));
#6626=CARTESIAN_POINT('Origin',(0.,0.,-5.));
#6627=CARTESIAN_POINT('',(-5.,59.,-5.));
#6628=CARTESIAN_POINT('Origin',(0.,59.,-5.));
#6629=CARTESIAN_POINT('',(28.,0.,-5.));
#6630=CARTESIAN_POINT('Origin',(0.,0.,-5.));
#6631=CARTESIAN_POINT('Origin',(0.,0.,6.5));
#6632=CARTESIAN_POINT('',(28.,0.,-6.5));
#6633=CARTESIAN_POINT('Origin',(0.,0.,-6.5));
#6634=CARTESIAN_POINT('',(28.,-3.42901103761259E-15,6.5));
#6635=CARTESIAN_POINT('Origin',(0.,0.,6.5));
#6636=CARTESIAN_POINT('',(25.,0.,6.5));
#6637=CARTESIAN_POINT('Origin',(0.,0.,6.5));
#6638=CARTESIAN_POINT('',(25.,0.,-6.5));
#6639=CARTESIAN_POINT('',(25.,-3.06161699786838E-15,6.5));
#6640=CARTESIAN_POINT('Origin',(0.,0.,-6.5));
#6641=CARTESIAN_POINT('Origin',(0.,0.,6.5));
#6642=CARTESIAN_POINT('',(28.,0.,6.5));
#6643=CARTESIAN_POINT('',(28.,-3.42901103761259E-15,6.5));
#6644=CARTESIAN_POINT('Origin',(0.,0.,6.5));
#6645=CARTESIAN_POINT('Origin',(0.,0.,6.5));
#6646=CARTESIAN_POINT('Origin',(0.,0.,-6.5));
#6647=CARTESIAN_POINT('Origin',(0.,59.,-15.));
#6648=CARTESIAN_POINT('',(-5.,59.,-15.));
#6649=CARTESIAN_POINT('Origin',(0.,0.,-7.38119784648294));
#6650=CARTESIAN_POINT('',(122.,0.,-7.38119784648294));
#6651=CARTESIAN_POINT('',(122.,-1.49406909495977E-14,-7.38119784648294));
#6652=CARTESIAN_POINT('',(-122.,-1.49406909495977E-14,-7.38119784648294));
#6653=CARTESIAN_POINT('Origin',(0.,0.,-7.38119784648294));
#6654=CARTESIAN_POINT('Origin',(0.,0.,-7.38119784648294));
#6655=CARTESIAN_POINT('Origin',(0.,0.,12.));
#6656=CARTESIAN_POINT('',(-122.,-1.49406909495977E-14,7.38119784648294));
#6657=CARTESIAN_POINT('',(-130.,-1.59204083889156E-14,12.));
#6658=CARTESIAN_POINT('Origin',(0.,0.,7.38119784648294));
#6659=CARTESIAN_POINT('Origin',(0.,0.,15.));
#6660=CARTESIAN_POINT('',(-122.,-1.49406909495977E-14,15.));
#6661=CARTESIAN_POINT('',(0.,0.,0.));
#6662=CARTESIAN_POINT('Origin',(-506.719999999999,51.0306388527815,12.));
#6663=CARTESIAN_POINT('',(-506.719999999999,51.0306388527815,-12.));
#6664=CARTESIAN_POINT('',(-19.5199999999996,130.,-12.));
#6665=CARTESIAN_POINT('',(-506.719999999999,51.0306388527815,-12.));
#6666=CARTESIAN_POINT('',(-506.719999999999,51.0306388527815,12.));
#6667=CARTESIAN_POINT('',(-506.719999999999,51.0306388527815,-12.));
#6668=CARTESIAN_POINT('',(-19.5199999999996,130.,12.));
#6669=CARTESIAN_POINT('',(-506.719999999999,51.0306388527815,12.));
#6670=CARTESIAN_POINT('',(-19.5199999999996,130.,-12.));
#6671=CARTESIAN_POINT('Origin',(-506.719999999999,51.0306388527815,-12.));
#6672=CARTESIAN_POINT('',(-506.719999999999,43.0306388527815,-7.38119784648294));
#6673=CARTESIAN_POINT('',(-19.5199999999996,122.,-7.38119784648294));
#6674=CARTESIAN_POINT('',(-506.719999999999,43.0306388527815,-7.38119784648294));
#6675=CARTESIAN_POINT('',(-506.719999999999,43.0306388527815,-7.38119784648295));
#6676=CARTESIAN_POINT('',(-19.5199999999996,122.,-7.38119784648295));
#6677=CARTESIAN_POINT('Origin',(-506.719999999999,43.0306388527815,7.38119784648301));
#6678=CARTESIAN_POINT('',(-506.719999999999,43.0306388527815,7.38119784648301));
#6679=CARTESIAN_POINT('',(-19.5199999999996,122.,7.38119784648301));
#6680=CARTESIAN_POINT('',(-506.719999999999,43.0306388527815,7.38119784648301));
#6681=CARTESIAN_POINT('',(-506.719999999999,43.0306388527815,7.38119784648301));
#6682=CARTESIAN_POINT('',(-19.5199999999996,122.,7.38119784648301));
#6683=CARTESIAN_POINT('Origin',(-499.999999999999,1.45487256761396E-12,
0.));
#6684=CARTESIAN_POINT('',(-509.743491796554,-50.5405665711541,-12.));
#6685=CARTESIAN_POINT('Origin',(-499.999999999999,1.45487256761396E-12,
-12.));
#6686=CARTESIAN_POINT('',(-509.743491796554,-50.5405665711541,12.));
#6687=CARTESIAN_POINT('',(-509.743491796554,-50.5405665711534,-12.));
#6688=CARTESIAN_POINT('Origin',(-499.999999999999,1.45487256761396E-12,
12.));
#6689=CARTESIAN_POINT('Ctrl Pts',(-507.216472239843,-42.9501665711535,-7.38119784648294));
#6690=CARTESIAN_POINT('Ctrl Pts',(-571.454108893077,-32.1569809174214,-7.38119784648294));
#6691=CARTESIAN_POINT('Ctrl Pts',(-571.077993559862,32.97999288859,-7.38119784648294));
#6692=CARTESIAN_POINT('Ctrl Pts',(-506.719999999999,43.0306388527815,-7.38119784648294));
#6693=CARTESIAN_POINT('Ctrl Pts',(-509.743491796554,-50.5405665711535,-12.));
#6694=CARTESIAN_POINT('Ctrl Pts',(-585.333572367437,-35.9678900083305,-12.));
#6695=CARTESIAN_POINT('Ctrl Pts',(-583.043048279138,40.9799928885899,-12.));
#6696=CARTESIAN_POINT('Ctrl Pts',(-506.719999999999,51.0306388527815,-12.));
#6697=CARTESIAN_POINT('',(-507.216472239843,-42.9501665711541,-7.38119784648294));
#6698=CARTESIAN_POINT('Origin',(-499.999999999999,1.45487256761396E-12,
-7.38119784648294));
#6699=CARTESIAN_POINT('',(-507.216472239843,-42.9501665711539,-7.38119784648324));
#6700=CARTESIAN_POINT('Origin',(-499.999999999999,1.45487256761396E-12,
0.));
#6701=CARTESIAN_POINT('',(-507.216472239843,-42.9501665711541,7.38119784648301));
#6702=CARTESIAN_POINT('Origin',(-499.999999999999,1.45487256761396E-12,
7.38119784648301));
#6703=CARTESIAN_POINT('',(-507.216472239843,-42.9501665711534,7.38119784648301));
#6704=CARTESIAN_POINT('Ctrl Pts',(-509.743491796554,-50.5405665711535,12.));
#6705=CARTESIAN_POINT('Ctrl Pts',(-585.333572367437,-35.9678900083305,12.));
#6706=CARTESIAN_POINT('Ctrl Pts',(-583.043048279138,40.9799928885899,12.));
#6707=CARTESIAN_POINT('Ctrl Pts',(-506.719999999999,51.0306388527815,12.));
#6708=CARTESIAN_POINT('Ctrl Pts',(-507.216472239843,-42.9501665711535,7.38119784648301));
#6709=CARTESIAN_POINT('Ctrl Pts',(-571.454108893077,-32.1569809174214,7.38119784648301));
#6710=CARTESIAN_POINT('Ctrl Pts',(-571.077993559862,32.97999288859,7.38119784648301));
#6711=CARTESIAN_POINT('Ctrl Pts',(-506.719999999999,43.0306388527815,7.38119784648301));
#6712=CARTESIAN_POINT('',(-506.719999999999,51.0306388527815,12.));
#6713=CARTESIAN_POINT('',(-509.743491796554,-50.5405665711539,12.0000000000003));
#6714=CARTESIAN_POINT('Origin',(-22.5434917965546,-129.509927718375,12.));
#6715=CARTESIAN_POINT('',(-22.5434917965544,-129.509927718374,-12.));
#6716=CARTESIAN_POINT('',(-22.5434917965545,-129.509927718375,-12.));
#6717=CARTESIAN_POINT('',(-22.5434917965544,-129.509927718374,12.));
#6718=CARTESIAN_POINT('',(-22.5434917965546,-129.509927718375,-12.));
#6719=CARTESIAN_POINT('',(-22.5434917965545,-129.509927718375,12.));
#6720=CARTESIAN_POINT('Origin',(-22.5434917965546,-129.509927718375,-12.));
#6721=CARTESIAN_POINT('',(-20.0164722398434,-121.919527718374,-7.38119784648294));
#6722=CARTESIAN_POINT('',(-20.0164722398435,-121.919527718375,-7.38119784648294));
#6723=CARTESIAN_POINT('',(-20.0164722398434,-121.919527718374,-7.38119784648264));
#6724=CARTESIAN_POINT('Origin',(-20.0164722398436,-121.919527718375,7.38119784648301));
#6725=CARTESIAN_POINT('',(-20.0164722398434,-121.919527718374,7.38119784648301));
#6726=CARTESIAN_POINT('',(-20.0164722398435,-121.919527718375,7.38119784648301));
#6727=CARTESIAN_POINT('',(-20.0164722398436,-121.919527718375,7.38119784648301));
#6728=CARTESIAN_POINT('Origin',(-22.5434917965546,-129.509927718375,12.));
#6729=CARTESIAN_POINT('',(-22.5434917965544,-129.509927718374,11.9999999999997));
#6730=CARTESIAN_POINT('Origin',(1.66533453693773E-13,3.77520255149252E-13,
0.));
#6731=CARTESIAN_POINT('Origin',(1.66533453693773E-13,3.77520255149252E-13,
-12.));
#6732=CARTESIAN_POINT('Origin',(1.66533453693773E-13,3.77520255149252E-13,
12.));
#6733=CARTESIAN_POINT('Ctrl Pts',(-19.5199999999996,122.,-7.38119784648294));
#6734=CARTESIAN_POINT('Ctrl Pts',(61.4089525234421,134.948632403751,-7.38119784648294));
#6735=CARTESIAN_POINT('Ctrl Pts',(123.718292795081,81.706651293145,-7.38119784648294));
#6736=CARTESIAN_POINT('Ctrl Pts',(123.55147574951,-0.251475880078228,-7.38119784648294));
#6737=CARTESIAN_POINT('Ctrl Pts',(123.384658703939,-82.2096030533015,-7.38119784648294));
#6738=CARTESIAN_POINT('Ctrl Pts',(60.8590988290158,-135.197496010055,-7.38119784648294));
#6739=CARTESIAN_POINT('Ctrl Pts',(-20.0164722398431,-121.919527718374,-7.38119784648294));
#6740=CARTESIAN_POINT('Ctrl Pts',(-19.5199999999996,130.,-12.));
#6741=CARTESIAN_POINT('Ctrl Pts',(66.7157690823563,142.948632403751,-12.));
#6742=CARTESIAN_POINT('Ctrl Pts',(132.464319559229,85.6651002104318,-12.));
#6743=CARTESIAN_POINT('Ctrl Pts',(131.448411864232,-1.53147588007823,-12.));
#6744=CARTESIAN_POINT('Ctrl Pts',(130.432504169234,-88.7280519705883,-12.));
#6745=CARTESIAN_POINT('Ctrl Pts',(63.3671868234026,-144.464199663587,-12.));
#6746=CARTESIAN_POINT('Ctrl Pts',(-22.5434917965542,-129.509927718374,-12.));
#6747=CARTESIAN_POINT('Origin',(1.66533453693773E-13,3.77520255149252E-13,
-7.38119784648294));
#6748=CARTESIAN_POINT('Origin',(1.66533453693773E-13,3.77520255149252E-13,
0.));
#6749=CARTESIAN_POINT('Origin',(1.66533453693773E-13,3.77520255149252E-13,
7.38119784648301));
#6750=CARTESIAN_POINT('Ctrl Pts',(-19.5199999999996,130.,12.));
#6751=CARTESIAN_POINT('Ctrl Pts',(66.7157690823563,142.948632403751,12.));
#6752=CARTESIAN_POINT('Ctrl Pts',(132.464319559229,85.6651002104318,12.));
#6753=CARTESIAN_POINT('Ctrl Pts',(131.448411864232,-1.53147588007823,12.));
#6754=CARTESIAN_POINT('Ctrl Pts',(130.432504169234,-88.7280519705883,12.));
#6755=CARTESIAN_POINT('Ctrl Pts',(63.3671868234026,-144.464199663587,12.));
#6756=CARTESIAN_POINT('Ctrl Pts',(-22.5434917965542,-129.509927718374,12.));
#6757=CARTESIAN_POINT('Ctrl Pts',(-19.5199999999996,122.,7.38119784648301));
#6758=CARTESIAN_POINT('Ctrl Pts',(61.4089525234421,134.948632403751,7.38119784648302));
#6759=CARTESIAN_POINT('Ctrl Pts',(123.718292795081,81.706651293145,7.38119784648302));
#6760=CARTESIAN_POINT('Ctrl Pts',(123.55147574951,-0.251475880078228,7.38119784648301));
#6761=CARTESIAN_POINT('Ctrl Pts',(123.384658703939,-82.2096030533015,7.38119784648302));
#6762=CARTESIAN_POINT('Ctrl Pts',(60.8590988290158,-135.197496010055,7.38119784648302));
#6763=CARTESIAN_POINT('Ctrl Pts',(-20.0164722398431,-121.919527718374,7.38119784648301));
#6764=CARTESIAN_POINT('',(-19.5199999999996,130.,12.));
#6765=CARTESIAN_POINT('Origin',(-506.719999999999,51.0306388527815,12.));
#6766=CARTESIAN_POINT('',(0.,0.,0.));
#6767=CARTESIAN_POINT('',(275.,542.,-3.03576608295941E-15));
#6768=CARTESIAN_POINT('',(275.,260.,2.79182059415017E-15));
#6769=CARTESIAN_POINT('',(275.,513.,1.38777878078145E-14));
#6770=CARTESIAN_POINT('',(275.,181.301456,1.60461921527855E-14));
#6771=CARTESIAN_POINT('',(275.,181.301456,-3.60822483003176E-13));
#6772=UNCERTAINTY_MEASURE_WITH_UNIT(LENGTH_MEASURE(0.01),#6790,
'DISTANCE_ACCURACY_VALUE',
'Maximum model space distance between geometric entities at asserted c
onnectivities');
#6773=UNCERTAINTY_MEASURE_WITH_UNIT(LENGTH_MEASURE(0.01),#6790,
'DISTANCE_ACCURACY_VALUE',
'Maximum model space distance between geometric entities at asserted c
onnectivities');
#6774=UNCERTAINTY_MEASURE_WITH_UNIT(LENGTH_MEASURE(0.01),#6790,
'DISTANCE_ACCURACY_VALUE',
'Maximum model space distance between geometric entities at asserted c
onnectivities');
#6775=UNCERTAINTY_MEASURE_WITH_UNIT(LENGTH_MEASURE(0.01),#6790,
'DISTANCE_ACCURACY_VALUE',
'Maximum model space distance between geometric entities at asserted c
onnectivities');
#6776=UNCERTAINTY_MEASURE_WITH_UNIT(LENGTH_MEASURE(0.01),#6790,
'DISTANCE_ACCURACY_VALUE',
'Maximum model space distance between geometric entities at asserted c
onnectivities');
#6777=UNCERTAINTY_MEASURE_WITH_UNIT(LENGTH_MEASURE(0.01),#6790,
'DISTANCE_ACCURACY_VALUE',
'Maximum model space distance between geometric entities at asserted c
onnectivities');
#6778=UNCERTAINTY_MEASURE_WITH_UNIT(LENGTH_MEASURE(0.01),#6790,
'DISTANCE_ACCURACY_VALUE',
'Maximum model space distance between geometric entities at asserted c
onnectivities');
#6779=UNCERTAINTY_MEASURE_WITH_UNIT(LENGTH_MEASURE(0.01),#6790,
'DISTANCE_ACCURACY_VALUE',
'Maximum model space distance between geometric entities at asserted c
onnectivities');
#6780=UNCERTAINTY_MEASURE_WITH_UNIT(LENGTH_MEASURE(0.01),#6790,
'DISTANCE_ACCURACY_VALUE',
'Maximum model space distance between geometric entities at asserted c
onnectivities');
#6781=(
GEOMETRIC_REPRESENTATION_CONTEXT(3)
GLOBAL_UNCERTAINTY_ASSIGNED_CONTEXT((#6772))
GLOBAL_UNIT_ASSIGNED_CONTEXT((#6790,#6792,#6793))
REPRESENTATION_CONTEXT('','3D')
);
#6782=(
GEOMETRIC_REPRESENTATION_CONTEXT(3)
GLOBAL_UNCERTAINTY_ASSIGNED_CONTEXT((#6773))
GLOBAL_UNIT_ASSIGNED_CONTEXT((#6790,#6792,#6793))
REPRESENTATION_CONTEXT('','3D')
);
#6783=(
GEOMETRIC_REPRESENTATION_CONTEXT(3)
GLOBAL_UNCERTAINTY_ASSIGNED_CONTEXT((#6774))
GLOBAL_UNIT_ASSIGNED_CONTEXT((#6790,#6792,#6793))
REPRESENTATION_CONTEXT('','3D')
);
#6784=(
GEOMETRIC_REPRESENTATION_CONTEXT(3)
GLOBAL_UNCERTAINTY_ASSIGNED_CONTEXT((#6775))
GLOBAL_UNIT_ASSIGNED_CONTEXT((#6790,#6792,#6793))
REPRESENTATION_CONTEXT('','3D')
);
#6785=(
GEOMETRIC_REPRESENTATION_CONTEXT(3)
GLOBAL_UNCERTAINTY_ASSIGNED_CONTEXT((#6776))
GLOBAL_UNIT_ASSIGNED_CONTEXT((#6790,#6792,#6793))
REPRESENTATION_CONTEXT('','3D')
);
#6786=(
GEOMETRIC_REPRESENTATION_CONTEXT(3)
GLOBAL_UNCERTAINTY_ASSIGNED_CONTEXT((#6777))
GLOBAL_UNIT_ASSIGNED_CONTEXT((#6790,#6792,#6793))
REPRESENTATION_CONTEXT('','3D')
);
#6787=(
GEOMETRIC_REPRESENTATION_CONTEXT(3)
GLOBAL_UNCERTAINTY_ASSIGNED_CONTEXT((#6778))
GLOBAL_UNIT_ASSIGNED_CONTEXT((#6790,#6792,#6793))
REPRESENTATION_CONTEXT('','3D')
);
#6788=(
GEOMETRIC_REPRESENTATION_CONTEXT(3)
GLOBAL_UNCERTAINTY_ASSIGNED_CONTEXT((#6779))
GLOBAL_UNIT_ASSIGNED_CONTEXT((#6790,#6792,#6793))
REPRESENTATION_CONTEXT('','3D')
);
#6789=(
GEOMETRIC_REPRESENTATION_CONTEXT(3)
GLOBAL_UNCERTAINTY_ASSIGNED_CONTEXT((#6780))
GLOBAL_UNIT_ASSIGNED_CONTEXT((#6790,#6792,#6793))
REPRESENTATION_CONTEXT('','3D')
);
#6790=(
LENGTH_UNIT()
NAMED_UNIT(*)
SI_UNIT(.MILLI.,.METRE.)
);
#6791=(
LENGTH_UNIT()
NAMED_UNIT(*)
SI_UNIT($,.METRE.)
);
#6792=(
NAMED_UNIT(*)
PLANE_ANGLE_UNIT()
SI_UNIT($,.RADIAN.)
);
#6793=(
NAMED_UNIT(*)
SI_UNIT($,.STERADIAN.)
SOLID_ANGLE_UNIT()
);
#6794=SHAPE_DEFINITION_REPRESENTATION(#6802,#6819);
#6795=SHAPE_DEFINITION_REPRESENTATION(#6803,#6820);
#6796=SHAPE_DEFINITION_REPRESENTATION(#6804,#6821);
#6797=SHAPE_DEFINITION_REPRESENTATION(#6805,#6822);
#6798=SHAPE_DEFINITION_REPRESENTATION(#6809,#6823);
#6799=SHAPE_DEFINITION_REPRESENTATION(#6810,#6824);
#6800=SHAPE_DEFINITION_REPRESENTATION(#6811,#6825);
#6801=SHAPE_DEFINITION_REPRESENTATION(#6812,#6826);
#6802=PRODUCT_DEFINITION_SHAPE('',$,#6828);
#6803=PRODUCT_DEFINITION_SHAPE('',$,#6829);
#6804=PRODUCT_DEFINITION_SHAPE('',$,#6830);
#6805=PRODUCT_DEFINITION_SHAPE('',$,#6831);
#6806=PRODUCT_DEFINITION_SHAPE($,$,#45);
#6807=PRODUCT_DEFINITION_SHAPE($,$,#46);
#6808=PRODUCT_DEFINITION_SHAPE($,$,#47);
#6809=PRODUCT_DEFINITION_SHAPE('',$,#6832);
#6810=PRODUCT_DEFINITION_SHAPE('',$,#6833);
#6811=PRODUCT_DEFINITION_SHAPE('',$,#6834);
#6812=PRODUCT_DEFINITION_SHAPE('',$,#6835);
#6813=PRODUCT_DEFINITION_SHAPE($,$,#48);
#6814=PRODUCT_DEFINITION_SHAPE($,$,#49);
#6815=PRODUCT_DEFINITION_SHAPE($,$,#50);
#6816=PRODUCT_DEFINITION_SHAPE($,$,#51);
#6817=PRODUCT_DEFINITION_SHAPE($,$,#52);
#6818=PRODUCT_DEFINITION_SHAPE($,$,#53);
#6819=SHAPE_REPRESENTATION('',(#4034,#4426,#4427,#4428,#4429,#4430,#4431),
#6781);
#6820=SHAPE_REPRESENTATION('',(#4035,#4284,#4285,#4286),#6782);
#6821=SHAPE_REPRESENTATION('',(#4036),#6783);
#6822=SHAPE_REPRESENTATION('',(#4225),#6784);
#6823=SHAPE_REPRESENTATION('',(#4287),#6785);
#6824=SHAPE_REPRESENTATION('',(#4309),#6786);
#6825=SHAPE_REPRESENTATION('',(#4352),#6787);
#6826=SHAPE_REPRESENTATION('',(#4405),#6788);
#6827=PRODUCT_DEFINITION_CONTEXT('part definition',#6853,'design');
#6828=PRODUCT_DEFINITION(
'MAT-064',
'MAT-064',#6836,
#6827);
#6829=PRODUCT_DEFINITION('Base Assembly','Base Assembly',#6837,#6827);
#6830=PRODUCT_DEFINITION('Bottom Base','Bottom Base',#6838,#6827);
#6831=PRODUCT_DEFINITION('Base Cover','Base Cover',#6839,#6827);
#6832=PRODUCT_DEFINITION('Major Shaft','Major Shaft',#6840,#6827);
#6833=PRODUCT_DEFINITION('Radial Ball Bearing','Radial Ball Bearing',#6841,
#6827);
#6834=PRODUCT_DEFINITION('Big Pulley','Big Pulley',#6842,#6827);
#6835=PRODUCT_DEFINITION('Belt','Belt',#6843,#6827);
#6836=PRODUCT_DEFINITION_FORMATION('',$,#6855);
#6837=PRODUCT_DEFINITION_FORMATION('',$,#6856);
#6838=PRODUCT_DEFINITION_FORMATION('',$,#6857);
#6839=PRODUCT_DEFINITION_FORMATION('',$,#6858);
#6840=PRODUCT_DEFINITION_FORMATION('',$,#6859);
#6841=PRODUCT_DEFINITION_FORMATION('',$,#6860);
#6842=PRODUCT_DEFINITION_FORMATION('',$,#6861);
#6843=PRODUCT_DEFINITION_FORMATION('',$,#6862);
#6844=PRODUCT_RELATED_PRODUCT_CATEGORY(
'MAT-064',
'MAT-064',(#6855));
#6845=PRODUCT_RELATED_PRODUCT_CATEGORY('Base Assembly','Base Assembly',
(#6856));
#6846=PRODUCT_RELATED_PRODUCT_CATEGORY('Bottom Base','Bottom Base',(#6857));
#6847=PRODUCT_RELATED_PRODUCT_CATEGORY('Base Cover','Base Cover',(#6858));
#6848=PRODUCT_RELATED_PRODUCT_CATEGORY('Major Shaft','Major Shaft',(#6859));
#6849=PRODUCT_RELATED_PRODUCT_CATEGORY('Radial Ball Bearing',
'Radial Ball Bearing',(#6860));
#6850=PRODUCT_RELATED_PRODUCT_CATEGORY('Big Pulley','Big Pulley',(#6861));
#6851=PRODUCT_RELATED_PRODUCT_CATEGORY('Belt','Belt',(#6862));
#6852=APPLICATION_PROTOCOL_DEFINITION('international standard',
'automotive_design',2009,#6853);
#6853=APPLICATION_CONTEXT(
'Core Data for Automotive Mechanical Design Process');
#6854=PRODUCT_CONTEXT('part definition',#6853,'mechanical');
#6855=PRODUCT(
'MAT-064',
'MAT-064',$,(#6854));
#6856=PRODUCT('Base Assembly','Base Assembly',$,(#6854));
#6857=PRODUCT('Bottom Base','Bottom Base',$,(#6854));
#6858=PRODUCT('Base Cover','Base Cover',$,(#6854));
#6859=PRODUCT('Major Shaft','Major Shaft',$,(#6854));
#6860=PRODUCT('Radial Ball Bearing','Radial Ball Bearing',$,(#6854));
#6861=PRODUCT('Big Pulley','Big Pulley',$,(#6854));
#6862=PRODUCT('Belt','Belt','Belt1-13__ DE    13309',(#6854));
#6863=PRESENTATION_STYLE_ASSIGNMENT((#6865));
#6864=PRESENTATION_STYLE_ASSIGNMENT((#6866));
#6865=SURFACE_STYLE_USAGE(.BOTH.,#6867);
#6866=SURFACE_STYLE_USAGE(.BOTH.,#6868);
#6867=SURFACE_SIDE_STYLE('',(#6869));
#6868=SURFACE_SIDE_STYLE('',(#6870));
#6869=SURFACE_STYLE_FILL_AREA(#6871);
#6870=SURFACE_STYLE_FILL_AREA(#6872);
#6871=FILL_AREA_STYLE('Steel - Satin',(#6873));
#6872=FILL_AREA_STYLE('Opaque(163,170,173)',(#6874));
#6873=FILL_AREA_STYLE_COLOUR('Steel - Satin',#6875);
#6874=FILL_AREA_STYLE_COLOUR('Opaque(163,170,173)',#6876);
#6875=COLOUR_RGB('Steel - Satin',0.627450980392157,0.627450980392157,0.627450980392157);
#6876=COLOUR_RGB('Opaque(163,170,173)',0.63921568627451,0.666666666666667,
0.67843137254902);
ENDSEC;
END-ISO-10303-21;
